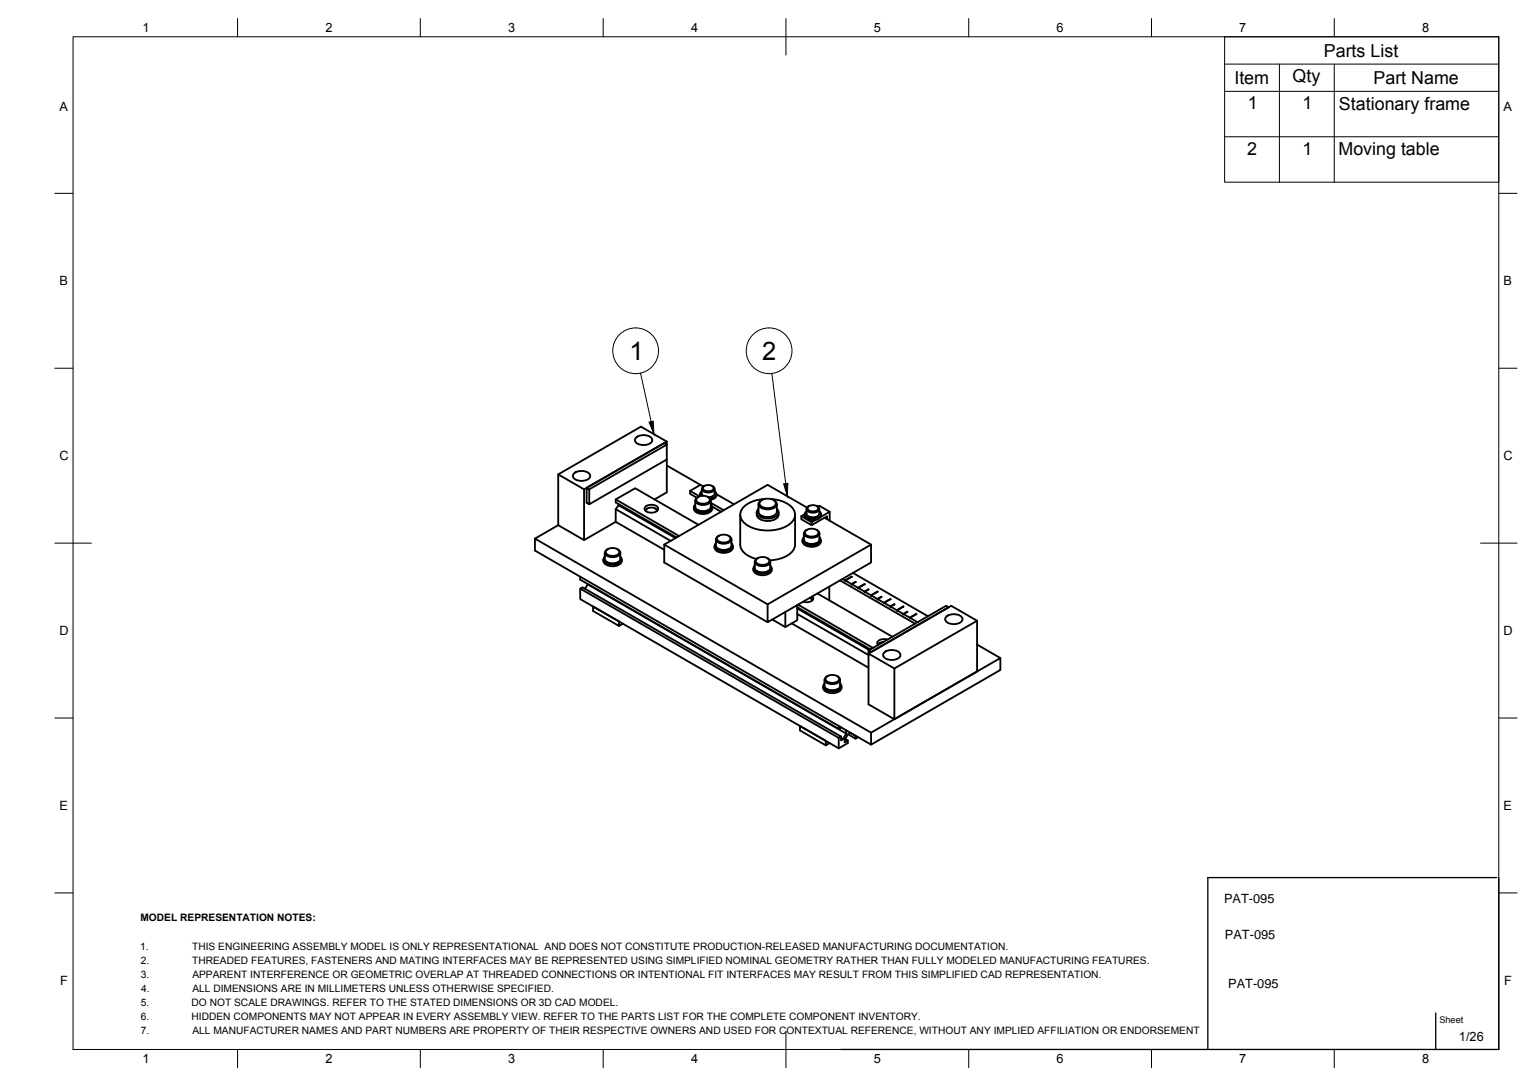
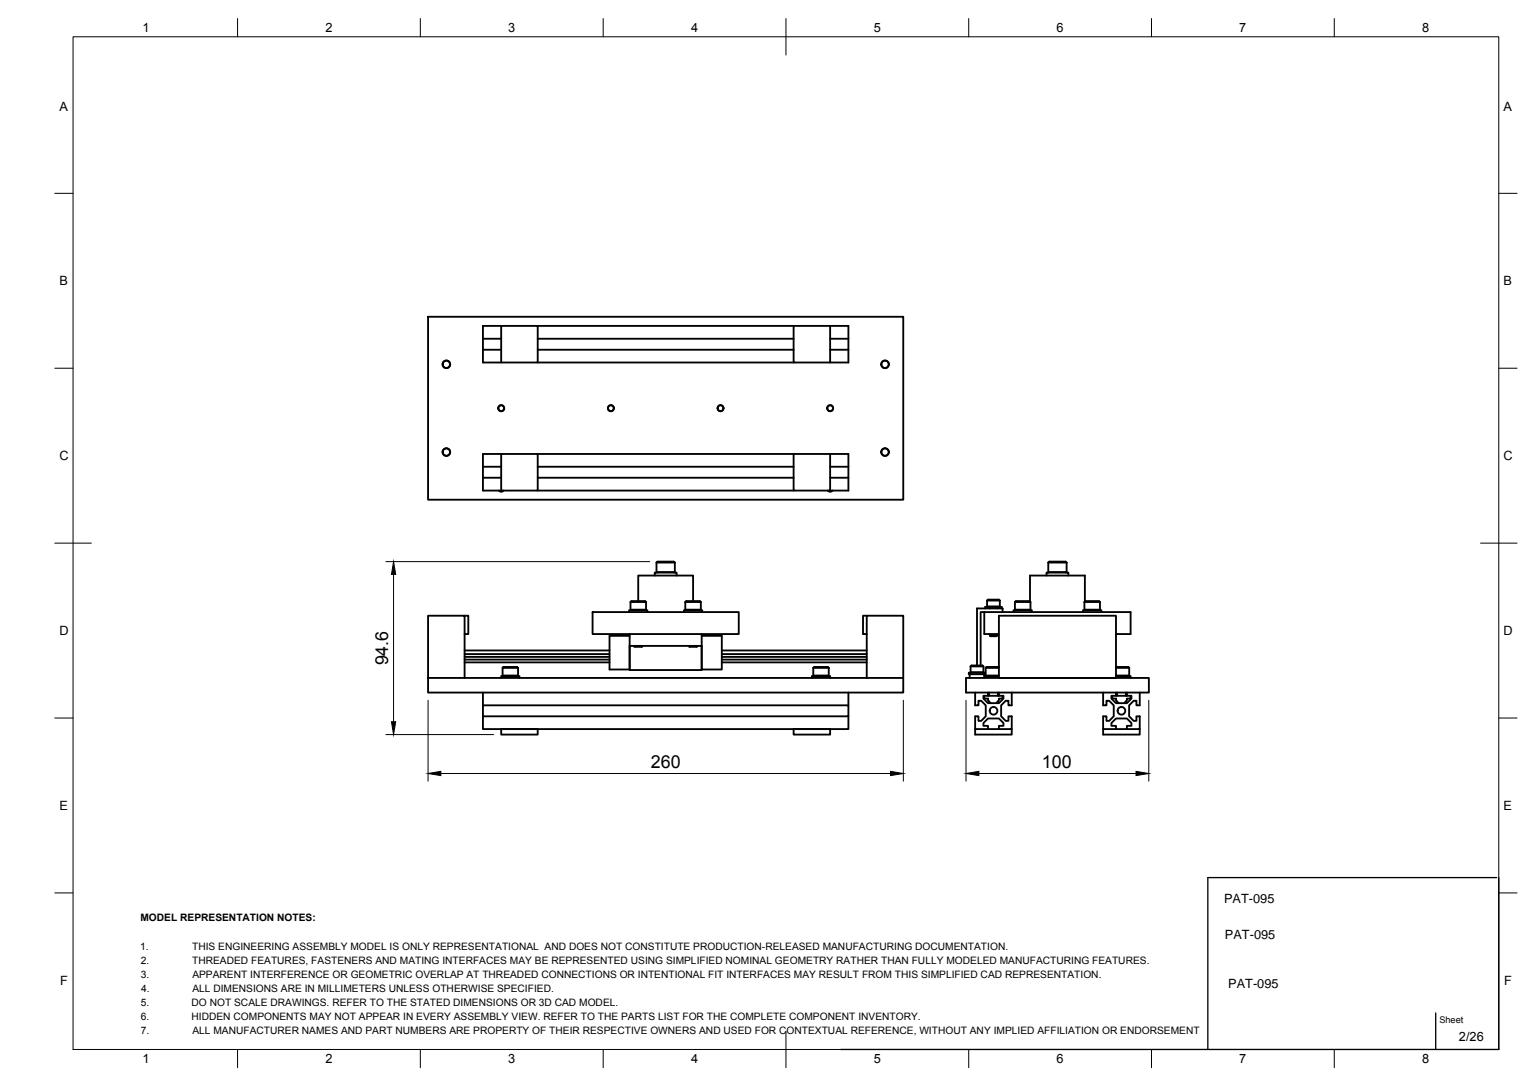
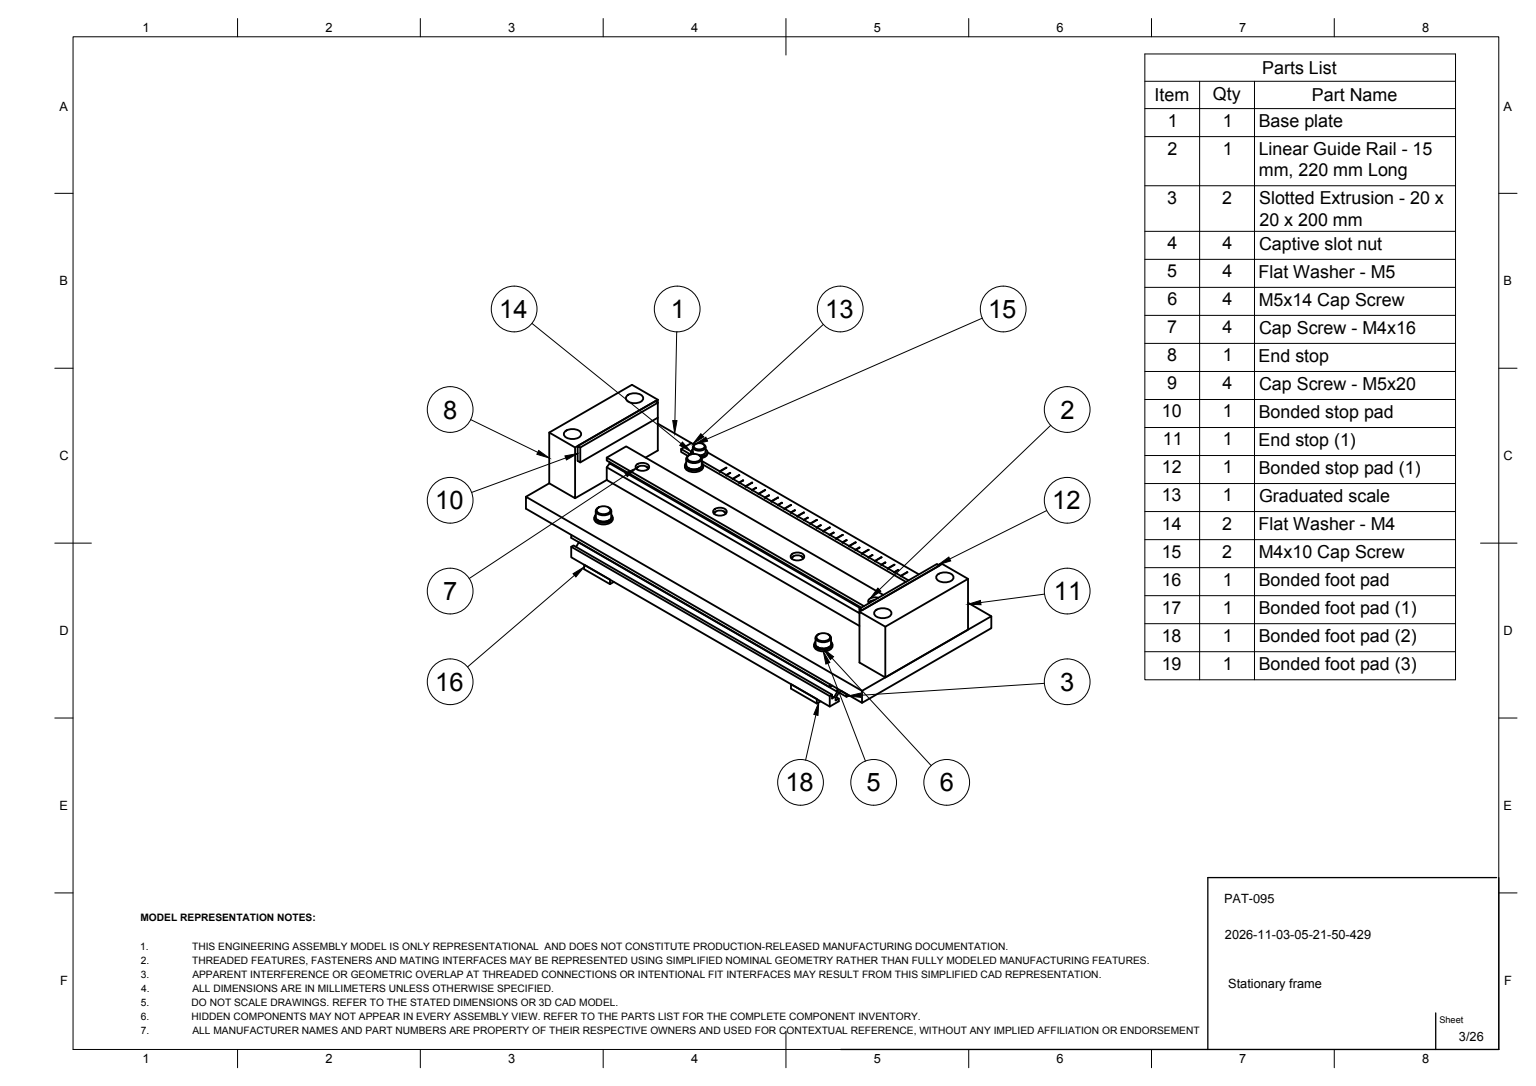
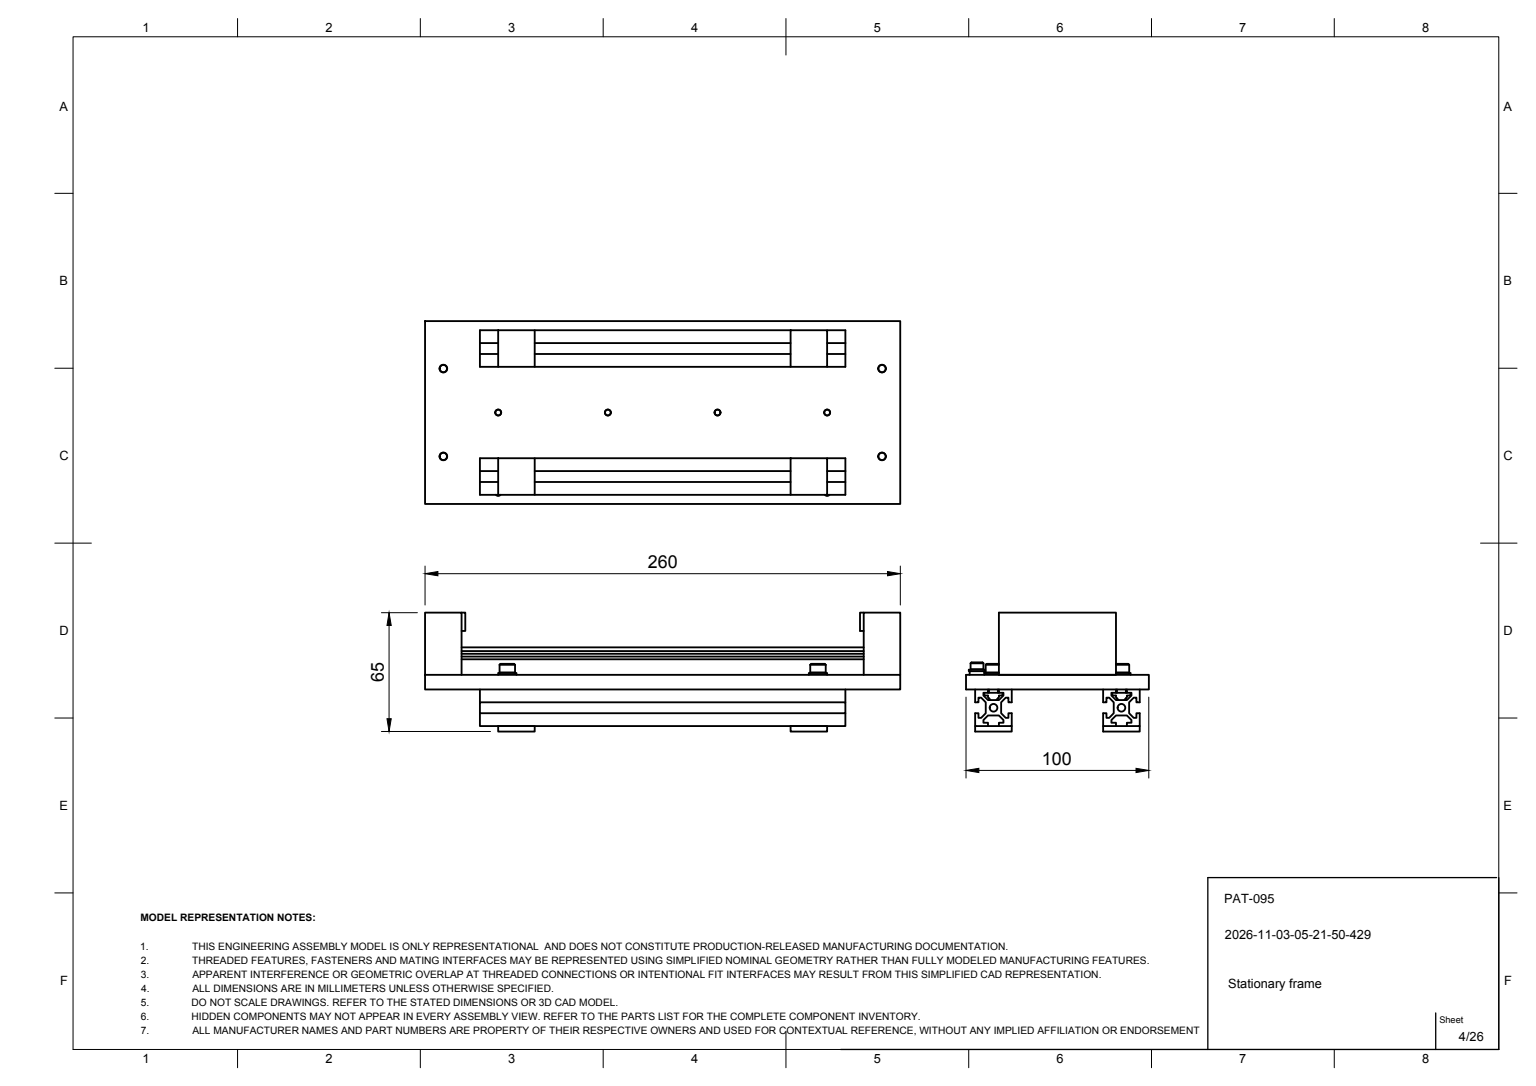
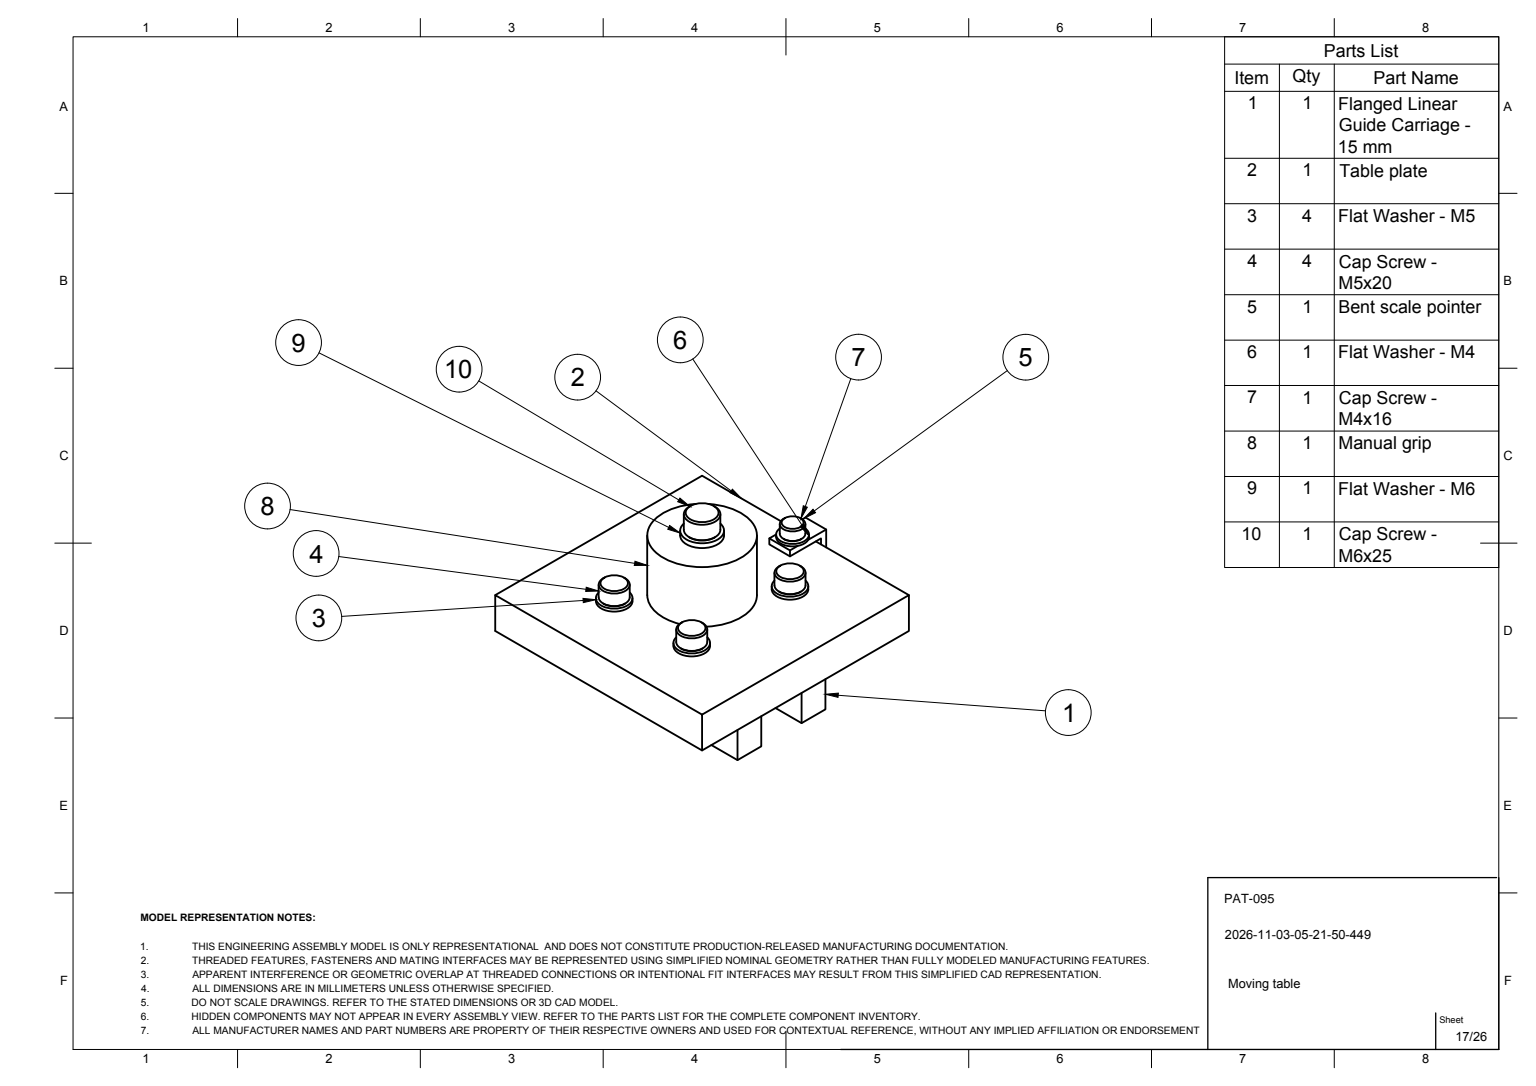
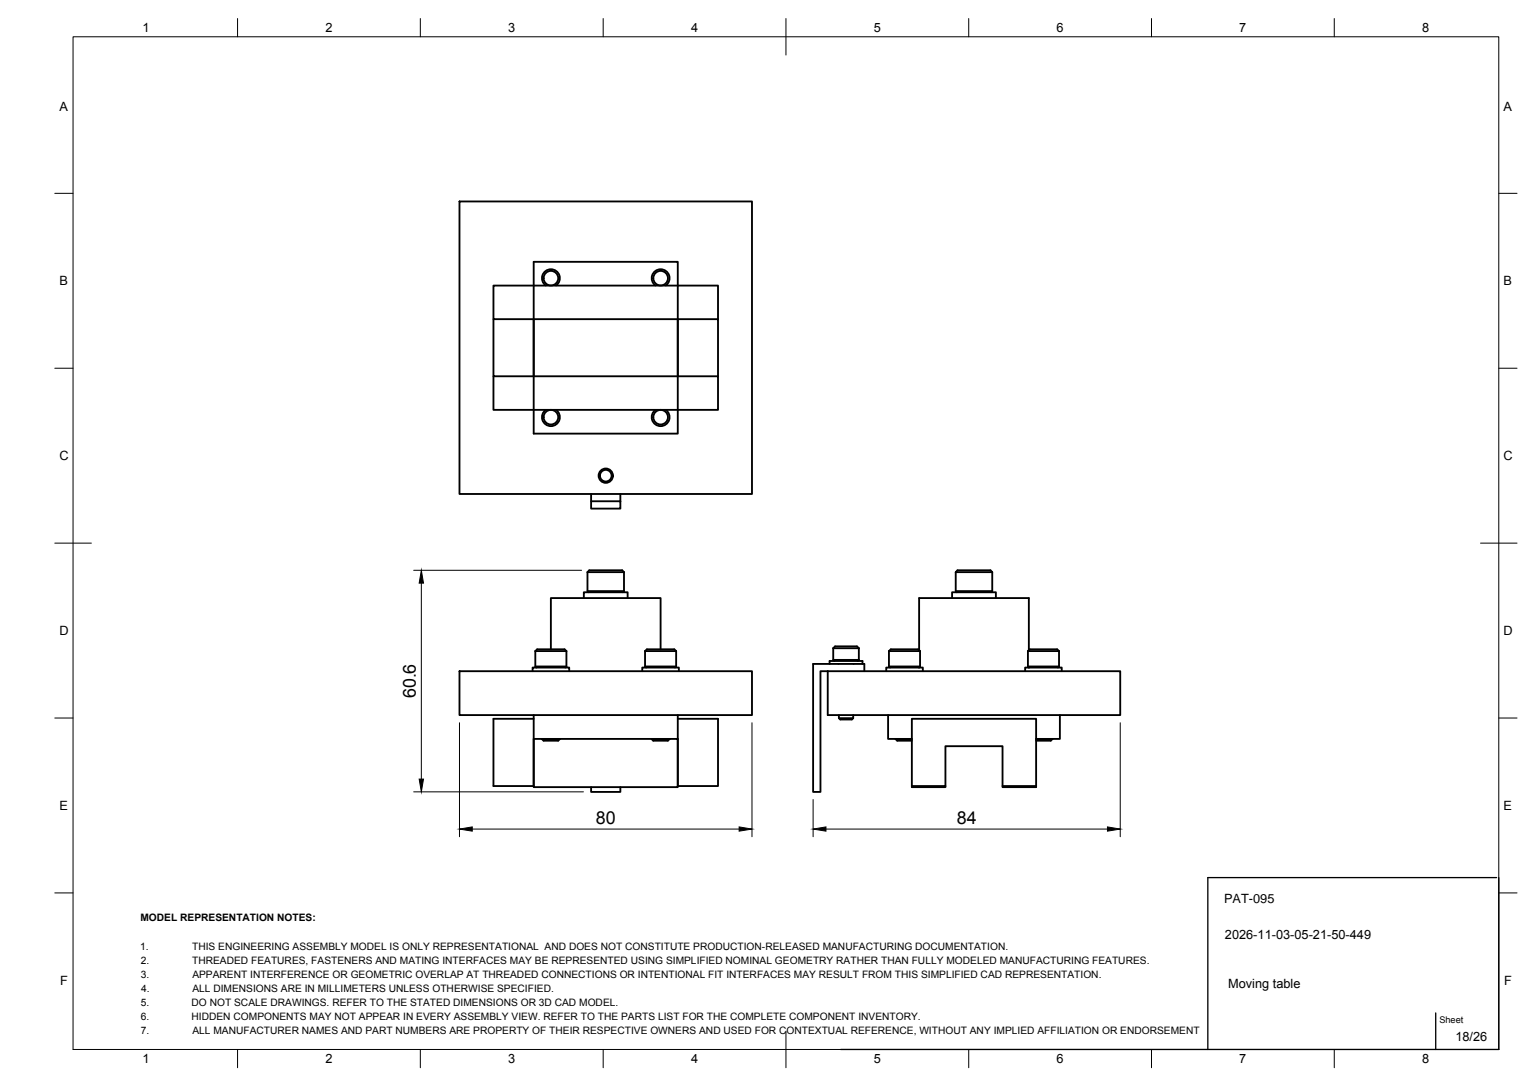
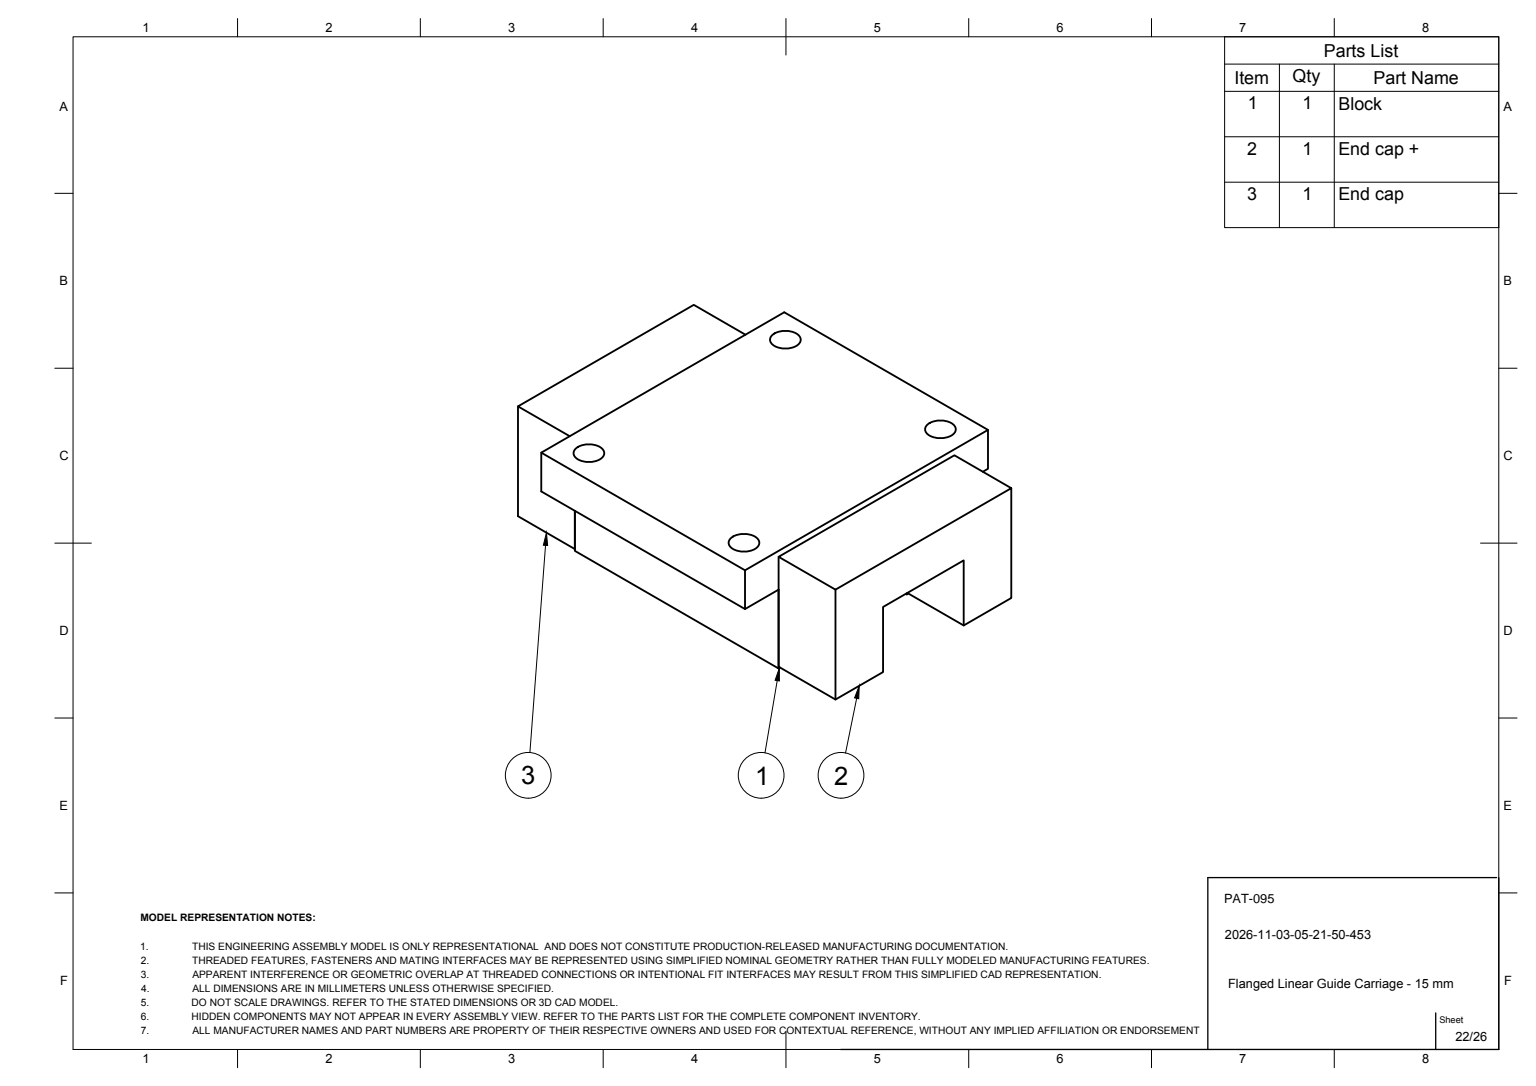
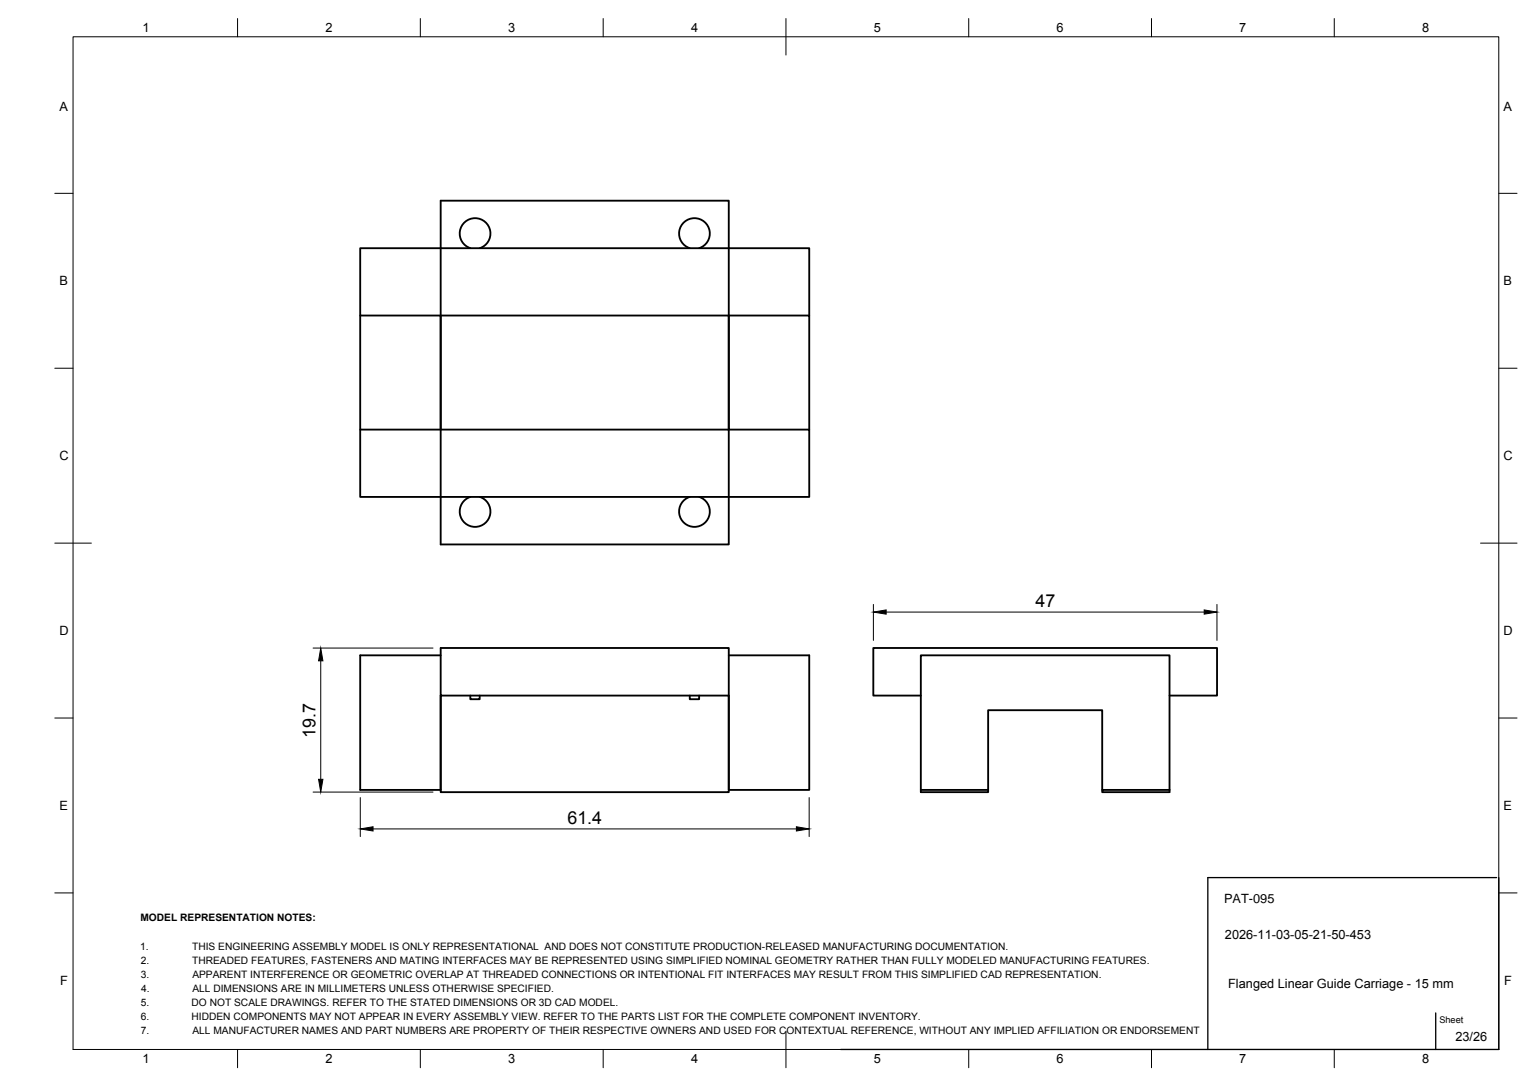
ISO-10303-21;
HEADER;
/* Generated by software containing ST-Developer
 * from STEP Tools, Inc. (www.steptools.com) 
 */

FILE_DESCRIPTION(
/* description */ ('Single-Axis Profile-Rail Linear Slide'),
/* implementation_level */ '2;1');

FILE_NAME(
/* name */ 'PAT-095',
/* time_stamp */ '2026-10-27T10:47:43-07:00',
/* author */ (''),
/* organization */ (''),
/* preprocessor_version */ 'ST-DEVELOPER v20.2',
/* originating_system */ 'Autodesk Translation Framework v15.17.0.0',
/* authorisation */ '');

FILE_SCHEMA (('AUTOMOTIVE_DESIGN { 1 0 10303 214 3 1 1 }'));
ENDSEC;

DATA;
#10=MECHANICAL_DESIGN_GEOMETRIC_PRESENTATION_REPRESENTATION('',(#329,#330,
#331,#332,#333,#334,#335,#336,#337,#338,#339,#340,#341,#342,#343,#344,#345,
#346,#347,#348,#349,#350,#351,#352,#353,#354,#355),#14478);
#11=ITEM_DEFINED_TRANSFORMATION($,$,#9393,#9454);
#12=ITEM_DEFINED_TRANSFORMATION($,$,#9432,#9455);
#13=ITEM_DEFINED_TRANSFORMATION($,$,#9443,#9456);
#14=ITEM_DEFINED_TRANSFORMATION($,$,#8921,#9531);
#15=ITEM_DEFINED_TRANSFORMATION($,$,#8970,#9532);
#16=ITEM_DEFINED_TRANSFORMATION($,$,#8991,#9533);
#17=ITEM_DEFINED_TRANSFORMATION($,$,#8998,#9534);
#18=ITEM_DEFINED_TRANSFORMATION($,$,#9019,#9535);
#19=ITEM_DEFINED_TRANSFORMATION($,$,#9026,#9536);
#20=ITEM_DEFINED_TRANSFORMATION($,$,#9155,#9537);
#21=ITEM_DEFINED_TRANSFORMATION($,$,#9162,#9538);
#22=ITEM_DEFINED_TRANSFORMATION($,$,#9169,#9539);
#23=ITEM_DEFINED_TRANSFORMATION($,$,#9176,#9540);
#24=ITEM_DEFINED_TRANSFORMATION($,$,#9183,#9541);
#25=ITEM_DEFINED_TRANSFORMATION($,$,#9226,#9542);
#26=ITEM_DEFINED_TRANSFORMATION($,$,#9226,#9543);
#27=ITEM_DEFINED_TRANSFORMATION($,$,#9276,#9544);
#28=ITEM_DEFINED_TRANSFORMATION($,$,#9457,#9545);
#29=ITEM_DEFINED_TRANSFORMATION($,$,#9297,#9546);
#30=ITEM_DEFINED_TRANSFORMATION($,$,#9276,#9547);
#31=ITEM_DEFINED_TRANSFORMATION($,$,#9457,#9548);
#32=ITEM_DEFINED_TRANSFORMATION($,$,#9297,#9549);
#33=ITEM_DEFINED_TRANSFORMATION($,$,#9276,#9550);
#34=ITEM_DEFINED_TRANSFORMATION($,$,#9457,#9551);
#35=ITEM_DEFINED_TRANSFORMATION($,$,#9297,#9552);
#36=ITEM_DEFINED_TRANSFORMATION($,$,#9276,#9553);
#37=ITEM_DEFINED_TRANSFORMATION($,$,#9457,#9554);
#38=ITEM_DEFINED_TRANSFORMATION($,$,#9297,#9555);
#39=ITEM_DEFINED_TRANSFORMATION($,$,#9505,#9556);
#40=ITEM_DEFINED_TRANSFORMATION($,$,#9505,#9557);
#41=ITEM_DEFINED_TRANSFORMATION($,$,#9505,#9558);
#42=ITEM_DEFINED_TRANSFORMATION($,$,#9505,#9559);
#43=ITEM_DEFINED_TRANSFORMATION($,$,#9468,#9560);
#44=ITEM_DEFINED_TRANSFORMATION($,$,#9468,#9561);
#45=ITEM_DEFINED_TRANSFORMATION($,$,#9468,#9562);
#46=ITEM_DEFINED_TRANSFORMATION($,$,#9468,#9563);
#47=ITEM_DEFINED_TRANSFORMATION($,$,#9494,#9564);
#48=ITEM_DEFINED_TRANSFORMATION($,$,#9321,#9565);
#49=ITEM_DEFINED_TRANSFORMATION($,$,#9494,#9566);
#50=ITEM_DEFINED_TRANSFORMATION($,$,#9321,#9567);
#51=ITEM_DEFINED_TRANSFORMATION($,$,#9346,#9603);
#52=ITEM_DEFINED_TRANSFORMATION($,$,#9371,#9604);
#53=ITEM_DEFINED_TRANSFORMATION($,$,#9383,#9605);
#54=ITEM_DEFINED_TRANSFORMATION($,$,#9392,#9606);
#55=ITEM_DEFINED_TRANSFORMATION($,$,#9457,#9607);
#56=ITEM_DEFINED_TRANSFORMATION($,$,#9468,#9608);
#57=ITEM_DEFINED_TRANSFORMATION($,$,#9457,#9609);
#58=ITEM_DEFINED_TRANSFORMATION($,$,#9468,#9610);
#59=ITEM_DEFINED_TRANSFORMATION($,$,#9457,#9611);
#60=ITEM_DEFINED_TRANSFORMATION($,$,#9468,#9612);
#61=ITEM_DEFINED_TRANSFORMATION($,$,#9457,#9613);
#62=ITEM_DEFINED_TRANSFORMATION($,$,#9468,#9614);
#63=ITEM_DEFINED_TRANSFORMATION($,$,#9494,#9615);
#64=ITEM_DEFINED_TRANSFORMATION($,$,#9505,#9616);
#65=ITEM_DEFINED_TRANSFORMATION($,$,#9568,#9617);
#66=ITEM_DEFINED_TRANSFORMATION($,$,#9577,#9618);
#67=ITEM_DEFINED_TRANSFORMATION($,$,#8920,#9619);
#68=ITEM_DEFINED_TRANSFORMATION($,$,#9345,#9620);
#69=(
REPRESENTATION_RELATIONSHIP($,$,#14625,#14624)
REPRESENTATION_RELATIONSHIP_WITH_TRANSFORMATION(#11)
SHAPE_REPRESENTATION_RELATIONSHIP()
);
#70=(
REPRESENTATION_RELATIONSHIP($,$,#14626,#14624)
REPRESENTATION_RELATIONSHIP_WITH_TRANSFORMATION(#12)
SHAPE_REPRESENTATION_RELATIONSHIP()
);
#71=(
REPRESENTATION_RELATIONSHIP($,$,#14627,#14624)
REPRESENTATION_RELATIONSHIP_WITH_TRANSFORMATION(#13)
SHAPE_REPRESENTATION_RELATIONSHIP()
);
#72=(
REPRESENTATION_RELATIONSHIP($,$,#14605,#14604)
REPRESENTATION_RELATIONSHIP_WITH_TRANSFORMATION(#14)
SHAPE_REPRESENTATION_RELATIONSHIP()
);
#73=(
REPRESENTATION_RELATIONSHIP($,$,#14606,#14604)
REPRESENTATION_RELATIONSHIP_WITH_TRANSFORMATION(#15)
SHAPE_REPRESENTATION_RELATIONSHIP()
);
#74=(
REPRESENTATION_RELATIONSHIP($,$,#14607,#14604)
REPRESENTATION_RELATIONSHIP_WITH_TRANSFORMATION(#16)
SHAPE_REPRESENTATION_RELATIONSHIP()
);
#75=(
REPRESENTATION_RELATIONSHIP($,$,#14608,#14604)
REPRESENTATION_RELATIONSHIP_WITH_TRANSFORMATION(#17)
SHAPE_REPRESENTATION_RELATIONSHIP()
);
#76=(
REPRESENTATION_RELATIONSHIP($,$,#14609,#14604)
REPRESENTATION_RELATIONSHIP_WITH_TRANSFORMATION(#18)
SHAPE_REPRESENTATION_RELATIONSHIP()
);
#77=(
REPRESENTATION_RELATIONSHIP($,$,#14610,#14604)
REPRESENTATION_RELATIONSHIP_WITH_TRANSFORMATION(#19)
SHAPE_REPRESENTATION_RELATIONSHIP()
);
#78=(
REPRESENTATION_RELATIONSHIP($,$,#14611,#14604)
REPRESENTATION_RELATIONSHIP_WITH_TRANSFORMATION(#20)
SHAPE_REPRESENTATION_RELATIONSHIP()
);
#79=(
REPRESENTATION_RELATIONSHIP($,$,#14612,#14604)
REPRESENTATION_RELATIONSHIP_WITH_TRANSFORMATION(#21)
SHAPE_REPRESENTATION_RELATIONSHIP()
);
#80=(
REPRESENTATION_RELATIONSHIP($,$,#14613,#14604)
REPRESENTATION_RELATIONSHIP_WITH_TRANSFORMATION(#22)
SHAPE_REPRESENTATION_RELATIONSHIP()
);
#81=(
REPRESENTATION_RELATIONSHIP($,$,#14614,#14604)
REPRESENTATION_RELATIONSHIP_WITH_TRANSFORMATION(#23)
SHAPE_REPRESENTATION_RELATIONSHIP()
);
#82=(
REPRESENTATION_RELATIONSHIP($,$,#14615,#14604)
REPRESENTATION_RELATIONSHIP_WITH_TRANSFORMATION(#24)
SHAPE_REPRESENTATION_RELATIONSHIP()
);
#83=(
REPRESENTATION_RELATIONSHIP($,$,#14616,#14604)
REPRESENTATION_RELATIONSHIP_WITH_TRANSFORMATION(#25)
SHAPE_REPRESENTATION_RELATIONSHIP()
);
#84=(
REPRESENTATION_RELATIONSHIP($,$,#14616,#14604)
REPRESENTATION_RELATIONSHIP_WITH_TRANSFORMATION(#26)
SHAPE_REPRESENTATION_RELATIONSHIP()
);
#85=(
REPRESENTATION_RELATIONSHIP($,$,#14617,#14604)
REPRESENTATION_RELATIONSHIP_WITH_TRANSFORMATION(#27)
SHAPE_REPRESENTATION_RELATIONSHIP()
);
#86=(
REPRESENTATION_RELATIONSHIP($,$,#14628,#14604)
REPRESENTATION_RELATIONSHIP_WITH_TRANSFORMATION(#28)
SHAPE_REPRESENTATION_RELATIONSHIP()
);
#87=(
REPRESENTATION_RELATIONSHIP($,$,#14618,#14604)
REPRESENTATION_RELATIONSHIP_WITH_TRANSFORMATION(#29)
SHAPE_REPRESENTATION_RELATIONSHIP()
);
#88=(
REPRESENTATION_RELATIONSHIP($,$,#14617,#14604)
REPRESENTATION_RELATIONSHIP_WITH_TRANSFORMATION(#30)
SHAPE_REPRESENTATION_RELATIONSHIP()
);
#89=(
REPRESENTATION_RELATIONSHIP($,$,#14628,#14604)
REPRESENTATION_RELATIONSHIP_WITH_TRANSFORMATION(#31)
SHAPE_REPRESENTATION_RELATIONSHIP()
);
#90=(
REPRESENTATION_RELATIONSHIP($,$,#14618,#14604)
REPRESENTATION_RELATIONSHIP_WITH_TRANSFORMATION(#32)
SHAPE_REPRESENTATION_RELATIONSHIP()
);
#91=(
REPRESENTATION_RELATIONSHIP($,$,#14617,#14604)
REPRESENTATION_RELATIONSHIP_WITH_TRANSFORMATION(#33)
SHAPE_REPRESENTATION_RELATIONSHIP()
);
#92=(
REPRESENTATION_RELATIONSHIP($,$,#14628,#14604)
REPRESENTATION_RELATIONSHIP_WITH_TRANSFORMATION(#34)
SHAPE_REPRESENTATION_RELATIONSHIP()
);
#93=(
REPRESENTATION_RELATIONSHIP($,$,#14618,#14604)
REPRESENTATION_RELATIONSHIP_WITH_TRANSFORMATION(#35)
SHAPE_REPRESENTATION_RELATIONSHIP()
);
#94=(
REPRESENTATION_RELATIONSHIP($,$,#14617,#14604)
REPRESENTATION_RELATIONSHIP_WITH_TRANSFORMATION(#36)
SHAPE_REPRESENTATION_RELATIONSHIP()
);
#95=(
REPRESENTATION_RELATIONSHIP($,$,#14628,#14604)
REPRESENTATION_RELATIONSHIP_WITH_TRANSFORMATION(#37)
SHAPE_REPRESENTATION_RELATIONSHIP()
);
#96=(
REPRESENTATION_RELATIONSHIP($,$,#14618,#14604)
REPRESENTATION_RELATIONSHIP_WITH_TRANSFORMATION(#38)
SHAPE_REPRESENTATION_RELATIONSHIP()
);
#97=(
REPRESENTATION_RELATIONSHIP($,$,#14631,#14604)
REPRESENTATION_RELATIONSHIP_WITH_TRANSFORMATION(#39)
SHAPE_REPRESENTATION_RELATIONSHIP()
);
#98=(
REPRESENTATION_RELATIONSHIP($,$,#14631,#14604)
REPRESENTATION_RELATIONSHIP_WITH_TRANSFORMATION(#40)
SHAPE_REPRESENTATION_RELATIONSHIP()
);
#99=(
REPRESENTATION_RELATIONSHIP($,$,#14631,#14604)
REPRESENTATION_RELATIONSHIP_WITH_TRANSFORMATION(#41)
SHAPE_REPRESENTATION_RELATIONSHIP()
);
#100=(
REPRESENTATION_RELATIONSHIP($,$,#14631,#14604)
REPRESENTATION_RELATIONSHIP_WITH_TRANSFORMATION(#42)
SHAPE_REPRESENTATION_RELATIONSHIP()
);
#101=(
REPRESENTATION_RELATIONSHIP($,$,#14629,#14604)
REPRESENTATION_RELATIONSHIP_WITH_TRANSFORMATION(#43)
SHAPE_REPRESENTATION_RELATIONSHIP()
);
#102=(
REPRESENTATION_RELATIONSHIP($,$,#14629,#14604)
REPRESENTATION_RELATIONSHIP_WITH_TRANSFORMATION(#44)
SHAPE_REPRESENTATION_RELATIONSHIP()
);
#103=(
REPRESENTATION_RELATIONSHIP($,$,#14629,#14604)
REPRESENTATION_RELATIONSHIP_WITH_TRANSFORMATION(#45)
SHAPE_REPRESENTATION_RELATIONSHIP()
);
#104=(
REPRESENTATION_RELATIONSHIP($,$,#14629,#14604)
REPRESENTATION_RELATIONSHIP_WITH_TRANSFORMATION(#46)
SHAPE_REPRESENTATION_RELATIONSHIP()
);
#105=(
REPRESENTATION_RELATIONSHIP($,$,#14630,#14604)
REPRESENTATION_RELATIONSHIP_WITH_TRANSFORMATION(#47)
SHAPE_REPRESENTATION_RELATIONSHIP()
);
#106=(
REPRESENTATION_RELATIONSHIP($,$,#14619,#14604)
REPRESENTATION_RELATIONSHIP_WITH_TRANSFORMATION(#48)
SHAPE_REPRESENTATION_RELATIONSHIP()
);
#107=(
REPRESENTATION_RELATIONSHIP($,$,#14630,#14604)
REPRESENTATION_RELATIONSHIP_WITH_TRANSFORMATION(#49)
SHAPE_REPRESENTATION_RELATIONSHIP()
);
#108=(
REPRESENTATION_RELATIONSHIP($,$,#14619,#14604)
REPRESENTATION_RELATIONSHIP_WITH_TRANSFORMATION(#50)
SHAPE_REPRESENTATION_RELATIONSHIP()
);
#109=(
REPRESENTATION_RELATIONSHIP($,$,#14621,#14620)
REPRESENTATION_RELATIONSHIP_WITH_TRANSFORMATION(#51)
SHAPE_REPRESENTATION_RELATIONSHIP()
);
#110=(
REPRESENTATION_RELATIONSHIP($,$,#14622,#14620)
REPRESENTATION_RELATIONSHIP_WITH_TRANSFORMATION(#52)
SHAPE_REPRESENTATION_RELATIONSHIP()
);
#111=(
REPRESENTATION_RELATIONSHIP($,$,#14623,#14620)
REPRESENTATION_RELATIONSHIP_WITH_TRANSFORMATION(#53)
SHAPE_REPRESENTATION_RELATIONSHIP()
);
#112=(
REPRESENTATION_RELATIONSHIP($,$,#14624,#14620)
REPRESENTATION_RELATIONSHIP_WITH_TRANSFORMATION(#54)
SHAPE_REPRESENTATION_RELATIONSHIP()
);
#113=(
REPRESENTATION_RELATIONSHIP($,$,#14628,#14620)
REPRESENTATION_RELATIONSHIP_WITH_TRANSFORMATION(#55)
SHAPE_REPRESENTATION_RELATIONSHIP()
);
#114=(
REPRESENTATION_RELATIONSHIP($,$,#14629,#14620)
REPRESENTATION_RELATIONSHIP_WITH_TRANSFORMATION(#56)
SHAPE_REPRESENTATION_RELATIONSHIP()
);
#115=(
REPRESENTATION_RELATIONSHIP($,$,#14628,#14620)
REPRESENTATION_RELATIONSHIP_WITH_TRANSFORMATION(#57)
SHAPE_REPRESENTATION_RELATIONSHIP()
);
#116=(
REPRESENTATION_RELATIONSHIP($,$,#14629,#14620)
REPRESENTATION_RELATIONSHIP_WITH_TRANSFORMATION(#58)
SHAPE_REPRESENTATION_RELATIONSHIP()
);
#117=(
REPRESENTATION_RELATIONSHIP($,$,#14628,#14620)
REPRESENTATION_RELATIONSHIP_WITH_TRANSFORMATION(#59)
SHAPE_REPRESENTATION_RELATIONSHIP()
);
#118=(
REPRESENTATION_RELATIONSHIP($,$,#14629,#14620)
REPRESENTATION_RELATIONSHIP_WITH_TRANSFORMATION(#60)
SHAPE_REPRESENTATION_RELATIONSHIP()
);
#119=(
REPRESENTATION_RELATIONSHIP($,$,#14628,#14620)
REPRESENTATION_RELATIONSHIP_WITH_TRANSFORMATION(#61)
SHAPE_REPRESENTATION_RELATIONSHIP()
);
#120=(
REPRESENTATION_RELATIONSHIP($,$,#14629,#14620)
REPRESENTATION_RELATIONSHIP_WITH_TRANSFORMATION(#62)
SHAPE_REPRESENTATION_RELATIONSHIP()
);
#121=(
REPRESENTATION_RELATIONSHIP($,$,#14630,#14620)
REPRESENTATION_RELATIONSHIP_WITH_TRANSFORMATION(#63)
SHAPE_REPRESENTATION_RELATIONSHIP()
);
#122=(
REPRESENTATION_RELATIONSHIP($,$,#14631,#14620)
REPRESENTATION_RELATIONSHIP_WITH_TRANSFORMATION(#64)
SHAPE_REPRESENTATION_RELATIONSHIP()
);
#123=(
REPRESENTATION_RELATIONSHIP($,$,#14632,#14620)
REPRESENTATION_RELATIONSHIP_WITH_TRANSFORMATION(#65)
SHAPE_REPRESENTATION_RELATIONSHIP()
);
#124=(
REPRESENTATION_RELATIONSHIP($,$,#14633,#14620)
REPRESENTATION_RELATIONSHIP_WITH_TRANSFORMATION(#66)
SHAPE_REPRESENTATION_RELATIONSHIP()
);
#125=(
REPRESENTATION_RELATIONSHIP($,$,#14604,#14603)
REPRESENTATION_RELATIONSHIP_WITH_TRANSFORMATION(#67)
SHAPE_REPRESENTATION_RELATIONSHIP()
);
#126=(
REPRESENTATION_RELATIONSHIP($,$,#14620,#14603)
REPRESENTATION_RELATIONSHIP_WITH_TRANSFORMATION(#68)
SHAPE_REPRESENTATION_RELATIONSHIP()
);
#127=CONTEXT_DEPENDENT_SHAPE_REPRESENTATION(#69,#14539);
#128=CONTEXT_DEPENDENT_SHAPE_REPRESENTATION(#70,#14540);
#129=CONTEXT_DEPENDENT_SHAPE_REPRESENTATION(#71,#14541);
#130=CONTEXT_DEPENDENT_SHAPE_REPRESENTATION(#72,#14546);
#131=CONTEXT_DEPENDENT_SHAPE_REPRESENTATION(#73,#14547);
#132=CONTEXT_DEPENDENT_SHAPE_REPRESENTATION(#74,#14548);
#133=CONTEXT_DEPENDENT_SHAPE_REPRESENTATION(#75,#14549);
#134=CONTEXT_DEPENDENT_SHAPE_REPRESENTATION(#76,#14550);
#135=CONTEXT_DEPENDENT_SHAPE_REPRESENTATION(#77,#14551);
#136=CONTEXT_DEPENDENT_SHAPE_REPRESENTATION(#78,#14552);
#137=CONTEXT_DEPENDENT_SHAPE_REPRESENTATION(#79,#14553);
#138=CONTEXT_DEPENDENT_SHAPE_REPRESENTATION(#80,#14554);
#139=CONTEXT_DEPENDENT_SHAPE_REPRESENTATION(#81,#14555);
#140=CONTEXT_DEPENDENT_SHAPE_REPRESENTATION(#82,#14556);
#141=CONTEXT_DEPENDENT_SHAPE_REPRESENTATION(#83,#14557);
#142=CONTEXT_DEPENDENT_SHAPE_REPRESENTATION(#84,#14558);
#143=CONTEXT_DEPENDENT_SHAPE_REPRESENTATION(#85,#14559);
#144=CONTEXT_DEPENDENT_SHAPE_REPRESENTATION(#86,#14560);
#145=CONTEXT_DEPENDENT_SHAPE_REPRESENTATION(#87,#14561);
#146=CONTEXT_DEPENDENT_SHAPE_REPRESENTATION(#88,#14562);
#147=CONTEXT_DEPENDENT_SHAPE_REPRESENTATION(#89,#14563);
#148=CONTEXT_DEPENDENT_SHAPE_REPRESENTATION(#90,#14564);
#149=CONTEXT_DEPENDENT_SHAPE_REPRESENTATION(#91,#14565);
#150=CONTEXT_DEPENDENT_SHAPE_REPRESENTATION(#92,#14566);
#151=CONTEXT_DEPENDENT_SHAPE_REPRESENTATION(#93,#14567);
#152=CONTEXT_DEPENDENT_SHAPE_REPRESENTATION(#94,#14568);
#153=CONTEXT_DEPENDENT_SHAPE_REPRESENTATION(#95,#14569);
#154=CONTEXT_DEPENDENT_SHAPE_REPRESENTATION(#96,#14570);
#155=CONTEXT_DEPENDENT_SHAPE_REPRESENTATION(#97,#14571);
#156=CONTEXT_DEPENDENT_SHAPE_REPRESENTATION(#98,#14572);
#157=CONTEXT_DEPENDENT_SHAPE_REPRESENTATION(#99,#14573);
#158=CONTEXT_DEPENDENT_SHAPE_REPRESENTATION(#100,#14574);
#159=CONTEXT_DEPENDENT_SHAPE_REPRESENTATION(#101,#14575);
#160=CONTEXT_DEPENDENT_SHAPE_REPRESENTATION(#102,#14576);
#161=CONTEXT_DEPENDENT_SHAPE_REPRESENTATION(#103,#14577);
#162=CONTEXT_DEPENDENT_SHAPE_REPRESENTATION(#104,#14578);
#163=CONTEXT_DEPENDENT_SHAPE_REPRESENTATION(#105,#14579);
#164=CONTEXT_DEPENDENT_SHAPE_REPRESENTATION(#106,#14580);
#165=CONTEXT_DEPENDENT_SHAPE_REPRESENTATION(#107,#14581);
#166=CONTEXT_DEPENDENT_SHAPE_REPRESENTATION(#108,#14582);
#167=CONTEXT_DEPENDENT_SHAPE_REPRESENTATION(#109,#14585);
#168=CONTEXT_DEPENDENT_SHAPE_REPRESENTATION(#110,#14586);
#169=CONTEXT_DEPENDENT_SHAPE_REPRESENTATION(#111,#14587);
#170=CONTEXT_DEPENDENT_SHAPE_REPRESENTATION(#112,#14588);
#171=CONTEXT_DEPENDENT_SHAPE_REPRESENTATION(#113,#14589);
#172=CONTEXT_DEPENDENT_SHAPE_REPRESENTATION(#114,#14590);
#173=CONTEXT_DEPENDENT_SHAPE_REPRESENTATION(#115,#14591);
#174=CONTEXT_DEPENDENT_SHAPE_REPRESENTATION(#116,#14592);
#175=CONTEXT_DEPENDENT_SHAPE_REPRESENTATION(#117,#14593);
#176=CONTEXT_DEPENDENT_SHAPE_REPRESENTATION(#118,#14594);
#177=CONTEXT_DEPENDENT_SHAPE_REPRESENTATION(#119,#14595);
#178=CONTEXT_DEPENDENT_SHAPE_REPRESENTATION(#120,#14596);
#179=CONTEXT_DEPENDENT_SHAPE_REPRESENTATION(#121,#14597);
#180=CONTEXT_DEPENDENT_SHAPE_REPRESENTATION(#122,#14598);
#181=CONTEXT_DEPENDENT_SHAPE_REPRESENTATION(#123,#14599);
#182=CONTEXT_DEPENDENT_SHAPE_REPRESENTATION(#124,#14600);
#183=CONTEXT_DEPENDENT_SHAPE_REPRESENTATION(#125,#14601);
#184=CONTEXT_DEPENDENT_SHAPE_REPRESENTATION(#126,#14602);
#185=NEXT_ASSEMBLY_USAGE_OCCURRENCE('Block:1','Block:1','Block:1',#14656,
#14657,'Block:1');
#186=NEXT_ASSEMBLY_USAGE_OCCURRENCE('End cap +:1','End cap +:1',
'End cap +:1',#14656,#14658,'End cap +:1');
#187=NEXT_ASSEMBLY_USAGE_OCCURRENCE('End cap:1','End cap:1','End cap:1',
#14656,#14659,'End cap:1');
#188=NEXT_ASSEMBLY_USAGE_OCCURRENCE('Base plate:1','Base plate:1',
'Base plate:1',#14636,#14637,'Base plate:1');
#189=NEXT_ASSEMBLY_USAGE_OCCURRENCE('End stop:1','End stop:1',
'End stop:1',#14636,#14638,'End stop:1');
#190=NEXT_ASSEMBLY_USAGE_OCCURRENCE('Bonded stop pad:1',
'Bonded stop pad:1','Bonded stop pad:1',#14636,#14639,
'Bonded stop pad:1');
#191=NEXT_ASSEMBLY_USAGE_OCCURRENCE('End stop (1):1','End stop (1):1',
'End stop (1):1',#14636,#14640,'End stop (1):1');
#192=NEXT_ASSEMBLY_USAGE_OCCURRENCE('Bonded stop pad (1):1',
'Bonded stop pad (1):1','Bonded stop pad (1):1',#14636,#14641,
'Bonded stop pad (1):1');
#193=NEXT_ASSEMBLY_USAGE_OCCURRENCE('Graduated scale:1',
'Graduated scale:1','Graduated scale:1',#14636,#14642,
'Graduated scale:1');
#194=NEXT_ASSEMBLY_USAGE_OCCURRENCE('Bonded foot pad:1',
'Bonded foot pad:1','Bonded foot pad:1',#14636,#14643,
'Bonded foot pad:1');
#195=NEXT_ASSEMBLY_USAGE_OCCURRENCE('Bonded foot pad (1):1',
'Bonded foot pad (1):1','Bonded foot pad (1):1',#14636,#14644,
'Bonded foot pad (1):1');
#196=NEXT_ASSEMBLY_USAGE_OCCURRENCE('Bonded foot pad (2):1',
'Bonded foot pad (2):1','Bonded foot pad (2):1',#14636,#14645,
'Bonded foot pad (2):1');
#197=NEXT_ASSEMBLY_USAGE_OCCURRENCE('Bonded foot pad (3):1',
'Bonded foot pad (3):1','Bonded foot pad (3):1',#14636,#14646,
'Bonded foot pad (3):1');
#198=NEXT_ASSEMBLY_USAGE_OCCURRENCE(
'Linear Guide Rail - 15 mm, 220 mm Long:2',
'Linear Guide Rail - 15 mm, 220 mm Long:2',
'Linear Guide Rail - 15 mm, 220 mm Long:2',#14636,#14647,
'Linear Guide Rail - 15 mm, 220 mm Long:2');
#199=NEXT_ASSEMBLY_USAGE_OCCURRENCE(
'Slotted Extrusion - 20 x 20 x 200 mm:2',
'Slotted Extrusion - 20 x 20 x 200 mm:2',
'Slotted Extrusion - 20 x 20 x 200 mm:2',#14636,#14648,
'Slotted Extrusion - 20 x 20 x 200 mm:2');
#200=NEXT_ASSEMBLY_USAGE_OCCURRENCE(
'Slotted Extrusion - 20 x 20 x 200 mm:3',
'Slotted Extrusion - 20 x 20 x 200 mm:3',
'Slotted Extrusion - 20 x 20 x 200 mm:3',#14636,#14648,
'Slotted Extrusion - 20 x 20 x 200 mm:3');
#201=NEXT_ASSEMBLY_USAGE_OCCURRENCE('Captive slot nut:2',
'Captive slot nut:2','Captive slot nut:2',#14636,#14649,
'Captive slot nut:2');
#202=NEXT_ASSEMBLY_USAGE_OCCURRENCE('Flat Washer - M5:2',
'Flat Washer - M5:2','Flat Washer - M5:2',#14636,#14660,
'Flat Washer - M5:2');
#203=NEXT_ASSEMBLY_USAGE_OCCURRENCE('M5x14 Cap Screw:2',
'M5x14 Cap Screw:2','M5x14 Cap Screw:2',#14636,#14650,
'M5x14 Cap Screw:2');
#204=NEXT_ASSEMBLY_USAGE_OCCURRENCE('Captive slot nut:3',
'Captive slot nut:3','Captive slot nut:3',#14636,#14649,
'Captive slot nut:3');
#205=NEXT_ASSEMBLY_USAGE_OCCURRENCE('Flat Washer - M5:3',
'Flat Washer - M5:3','Flat Washer - M5:3',#14636,#14660,
'Flat Washer - M5:3');
#206=NEXT_ASSEMBLY_USAGE_OCCURRENCE('M5x14 Cap Screw:3',
'M5x14 Cap Screw:3','M5x14 Cap Screw:3',#14636,#14650,
'M5x14 Cap Screw:3');
#207=NEXT_ASSEMBLY_USAGE_OCCURRENCE('Captive slot nut:4',
'Captive slot nut:4','Captive slot nut:4',#14636,#14649,
'Captive slot nut:4');
#208=NEXT_ASSEMBLY_USAGE_OCCURRENCE('Flat Washer - M5:4',
'Flat Washer - M5:4','Flat Washer - M5:4',#14636,#14660,
'Flat Washer - M5:4');
#209=NEXT_ASSEMBLY_USAGE_OCCURRENCE('M5x14 Cap Screw:4',
'M5x14 Cap Screw:4','M5x14 Cap Screw:4',#14636,#14650,
'M5x14 Cap Screw:4');
#210=NEXT_ASSEMBLY_USAGE_OCCURRENCE('Captive slot nut:5',
'Captive slot nut:5','Captive slot nut:5',#14636,#14649,
'Captive slot nut:5');
#211=NEXT_ASSEMBLY_USAGE_OCCURRENCE('Flat Washer - M5:5',
'Flat Washer - M5:5','Flat Washer - M5:5',#14636,#14660,
'Flat Washer - M5:5');
#212=NEXT_ASSEMBLY_USAGE_OCCURRENCE('M5x14 Cap Screw:5',
'M5x14 Cap Screw:5','M5x14 Cap Screw:5',#14636,#14650,
'M5x14 Cap Screw:5');
#213=NEXT_ASSEMBLY_USAGE_OCCURRENCE('Cap Screw - M4x16:2',
'Cap Screw - M4x16:2','Cap Screw - M4x16:2',#14636,#14663,
'Cap Screw - M4x16:2');
#214=NEXT_ASSEMBLY_USAGE_OCCURRENCE('Cap Screw - M4x16:3',
'Cap Screw - M4x16:3','Cap Screw - M4x16:3',#14636,#14663,
'Cap Screw - M4x16:3');
#215=NEXT_ASSEMBLY_USAGE_OCCURRENCE('Cap Screw - M4x16:4',
'Cap Screw - M4x16:4','Cap Screw - M4x16:4',#14636,#14663,
'Cap Screw - M4x16:4');
#216=NEXT_ASSEMBLY_USAGE_OCCURRENCE('Cap Screw - M4x16:5',
'Cap Screw - M4x16:5','Cap Screw - M4x16:5',#14636,#14663,
'Cap Screw - M4x16:5');
#217=NEXT_ASSEMBLY_USAGE_OCCURRENCE('Cap Screw - M5x20:6',
'Cap Screw - M5x20:6','Cap Screw - M5x20:6',#14636,#14661,
'Cap Screw - M5x20:6');
#218=NEXT_ASSEMBLY_USAGE_OCCURRENCE('Cap Screw - M5x20:7',
'Cap Screw - M5x20:7','Cap Screw - M5x20:7',#14636,#14661,
'Cap Screw - M5x20:7');
#219=NEXT_ASSEMBLY_USAGE_OCCURRENCE('Cap Screw - M5x20:8',
'Cap Screw - M5x20:8','Cap Screw - M5x20:8',#14636,#14661,
'Cap Screw - M5x20:8');
#220=NEXT_ASSEMBLY_USAGE_OCCURRENCE('Cap Screw - M5x20:9',
'Cap Screw - M5x20:9','Cap Screw - M5x20:9',#14636,#14661,
'Cap Screw - M5x20:9');
#221=NEXT_ASSEMBLY_USAGE_OCCURRENCE('Flat Washer - M4:2',
'Flat Washer - M4:2','Flat Washer - M4:2',#14636,#14662,
'Flat Washer - M4:2');
#222=NEXT_ASSEMBLY_USAGE_OCCURRENCE('M4x10 Cap Screw:2',
'M4x10 Cap Screw:2','M4x10 Cap Screw:2',#14636,#14651,
'M4x10 Cap Screw:2');
#223=NEXT_ASSEMBLY_USAGE_OCCURRENCE('Flat Washer - M4:3',
'Flat Washer - M4:3','Flat Washer - M4:3',#14636,#14662,
'Flat Washer - M4:3');
#224=NEXT_ASSEMBLY_USAGE_OCCURRENCE('M4x10 Cap Screw:3',
'M4x10 Cap Screw:3','M4x10 Cap Screw:3',#14636,#14651,
'M4x10 Cap Screw:3');
#225=NEXT_ASSEMBLY_USAGE_OCCURRENCE('Table plate:1','Table plate:1',
'Table plate:1',#14652,#14653,'Table plate:1');
#226=NEXT_ASSEMBLY_USAGE_OCCURRENCE('Bent scale pointer:1',
'Bent scale pointer:1','Bent scale pointer:1',#14652,#14654,
'Bent scale pointer:1');
#227=NEXT_ASSEMBLY_USAGE_OCCURRENCE('Manual grip:1','Manual grip:1',
'Manual grip:1',#14652,#14655,'Manual grip:1');
#228=NEXT_ASSEMBLY_USAGE_OCCURRENCE(
'Flanged Linear Guide Carriage - 15 mm:2',
'Flanged Linear Guide Carriage - 15 mm:2',
'Flanged Linear Guide Carriage - 15 mm:2',#14652,#14656,
'Flanged Linear Guide Carriage - 15 mm:2');
#229=NEXT_ASSEMBLY_USAGE_OCCURRENCE('Flat Washer - M5:6',
'Flat Washer - M5:6','Flat Washer - M5:6',#14652,#14660,
'Flat Washer - M5:6');
#230=NEXT_ASSEMBLY_USAGE_OCCURRENCE('Cap Screw - M5x20:2',
'Cap Screw - M5x20:2','Cap Screw - M5x20:2',#14652,#14661,
'Cap Screw - M5x20:2');
#231=NEXT_ASSEMBLY_USAGE_OCCURRENCE('Flat Washer - M5:7',
'Flat Washer - M5:7','Flat Washer - M5:7',#14652,#14660,
'Flat Washer - M5:7');
#232=NEXT_ASSEMBLY_USAGE_OCCURRENCE('Cap Screw - M5x20:3',
'Cap Screw - M5x20:3','Cap Screw - M5x20:3',#14652,#14661,
'Cap Screw - M5x20:3');
#233=NEXT_ASSEMBLY_USAGE_OCCURRENCE('Flat Washer - M5:8',
'Flat Washer - M5:8','Flat Washer - M5:8',#14652,#14660,
'Flat Washer - M5:8');
#234=NEXT_ASSEMBLY_USAGE_OCCURRENCE('Cap Screw - M5x20:4',
'Cap Screw - M5x20:4','Cap Screw - M5x20:4',#14652,#14661,
'Cap Screw - M5x20:4');
#235=NEXT_ASSEMBLY_USAGE_OCCURRENCE('Flat Washer - M5:9',
'Flat Washer - M5:9','Flat Washer - M5:9',#14652,#14660,
'Flat Washer - M5:9');
#236=NEXT_ASSEMBLY_USAGE_OCCURRENCE('Cap Screw - M5x20:5',
'Cap Screw - M5x20:5','Cap Screw - M5x20:5',#14652,#14661,
'Cap Screw - M5x20:5');
#237=NEXT_ASSEMBLY_USAGE_OCCURRENCE('Flat Washer - M4:4',
'Flat Washer - M4:4','Flat Washer - M4:4',#14652,#14662,
'Flat Washer - M4:4');
#238=NEXT_ASSEMBLY_USAGE_OCCURRENCE('Cap Screw - M4x16:6',
'Cap Screw - M4x16:6','Cap Screw - M4x16:6',#14652,#14663,
'Cap Screw - M4x16:6');
#239=NEXT_ASSEMBLY_USAGE_OCCURRENCE('Flat Washer - M6:2',
'Flat Washer - M6:2','Flat Washer - M6:2',#14652,#14664,
'Flat Washer - M6:2');
#240=NEXT_ASSEMBLY_USAGE_OCCURRENCE('Cap Screw - M6x25:2',
'Cap Screw - M6x25:2','Cap Screw - M6x25:2',#14652,#14665,
'Cap Screw - M6x25:2');
#241=NEXT_ASSEMBLY_USAGE_OCCURRENCE('Stationary frame:1',
'Stationary frame:1','Stationary frame:1',#14635,#14636,
'Stationary frame:1');
#242=NEXT_ASSEMBLY_USAGE_OCCURRENCE('Moving table:1','Moving table:1',
'Moving table:1',#14635,#14652,'Moving table:1');
#243=CONICAL_SURFACE('',#9310,0.4,0.785398163397448);
#244=CONICAL_SURFACE('',#9314,0.41,0.785398163397448);
#245=CONICAL_SURFACE('',#9318,0.26,0.463647609000806);
#246=CONICAL_SURFACE('',#9334,0.325,0.785398163397448);
#247=CONICAL_SURFACE('',#9338,0.335,0.785398163397448);
#248=CONICAL_SURFACE('',#9342,0.21,0.463647609000806);
#249=CONICAL_SURFACE('',#9458,0.275,0.785398163397449);
#250=CONICAL_SURFACE('',#9471,0.4,0.785398163397448);
#251=CONICAL_SURFACE('',#9475,0.41,0.785398163397448);
#252=CONICAL_SURFACE('',#9479,0.26,0.463647609000806);
#253=CONICAL_SURFACE('',#9483,0.225,0.785398163397448);
#254=CONICAL_SURFACE('',#9495,0.225,0.785398163397448);
#255=CONICAL_SURFACE('',#9508,0.325,0.785398163397448);
#256=CONICAL_SURFACE('',#9512,0.335,0.785398163397448);
#257=CONICAL_SURFACE('',#9516,0.21,0.463647609000806);
#258=CONICAL_SURFACE('',#9520,0.18,0.785398163397448);
#259=CONICAL_SURFACE('',#9580,0.475,0.785398163397449);
#260=CONICAL_SURFACE('',#9584,0.485,0.785398163397448);
#261=CONICAL_SURFACE('',#9588,0.31,0.463647609000806);
#262=CONICAL_SURFACE('',#9592,0.27,0.785398163397448);
#263=ORIENTED_CLOSED_SHELL('',*,#8602,.F.);
#264=ORIENTED_CLOSED_SHELL('',*,#8604,.F.);
#265=ORIENTED_CLOSED_SHELL('',*,#8614,.F.);
#266=ORIENTED_CLOSED_SHELL('',*,#8617,.F.);
#267=ORIENTED_CLOSED_SHELL('',*,#8620,.F.);
#268=BREP_WITH_VOIDS('Body1',#8603,(#263));
#269=BREP_WITH_VOIDS('Body1',#8605,(#264));
#270=BREP_WITH_VOIDS('Body1',#8613,(#265));
#271=BREP_WITH_VOIDS('Body1',#8616,(#266));
#272=BREP_WITH_VOIDS('Body1',#8619,(#267));
#273=ELLIPSE('',#9287,0.299389011154384,0.2117);
#274=ELLIPSE('',#9291,0.299389011154384,0.2117);
#275=SHAPE_REPRESENTATION_RELATIONSHIP('SRR','None',#14605,#302);
#276=SHAPE_REPRESENTATION_RELATIONSHIP('SRR','None',#14606,#303);
#277=SHAPE_REPRESENTATION_RELATIONSHIP('SRR','None',#14607,#304);
#278=SHAPE_REPRESENTATION_RELATIONSHIP('SRR','None',#14608,#305);
#279=SHAPE_REPRESENTATION_RELATIONSHIP('SRR','None',#14609,#306);
#280=SHAPE_REPRESENTATION_RELATIONSHIP('SRR','None',#14610,#307);
#281=SHAPE_REPRESENTATION_RELATIONSHIP('SRR','None',#14611,#308);
#282=SHAPE_REPRESENTATION_RELATIONSHIP('SRR','None',#14612,#309);
#283=SHAPE_REPRESENTATION_RELATIONSHIP('SRR','None',#14613,#310);
#284=SHAPE_REPRESENTATION_RELATIONSHIP('SRR','None',#14614,#311);
#285=SHAPE_REPRESENTATION_RELATIONSHIP('SRR','None',#14615,#312);
#286=SHAPE_REPRESENTATION_RELATIONSHIP('SRR','None',#14616,#313);
#287=SHAPE_REPRESENTATION_RELATIONSHIP('SRR','None',#14617,#314);
#288=SHAPE_REPRESENTATION_RELATIONSHIP('SRR','None',#14618,#315);
#289=SHAPE_REPRESENTATION_RELATIONSHIP('SRR','None',#14619,#316);
#290=SHAPE_REPRESENTATION_RELATIONSHIP('SRR','None',#14621,#317);
#291=SHAPE_REPRESENTATION_RELATIONSHIP('SRR','None',#14622,#318);
#292=SHAPE_REPRESENTATION_RELATIONSHIP('SRR','None',#14623,#319);
#293=SHAPE_REPRESENTATION_RELATIONSHIP('SRR','None',#14625,#320);
#294=SHAPE_REPRESENTATION_RELATIONSHIP('SRR','None',#14626,#321);
#295=SHAPE_REPRESENTATION_RELATIONSHIP('SRR','None',#14627,#322);
#296=SHAPE_REPRESENTATION_RELATIONSHIP('SRR','None',#14628,#323);
#297=SHAPE_REPRESENTATION_RELATIONSHIP('SRR','None',#14629,#324);
#298=SHAPE_REPRESENTATION_RELATIONSHIP('SRR','None',#14630,#325);
#299=SHAPE_REPRESENTATION_RELATIONSHIP('SRR','None',#14631,#326);
#300=SHAPE_REPRESENTATION_RELATIONSHIP('SRR','None',#14632,#327);
#301=SHAPE_REPRESENTATION_RELATIONSHIP('SRR','None',#14633,#328);
#302=ADVANCED_BREP_SHAPE_REPRESENTATION('',(#356),#14449);
#303=ADVANCED_BREP_SHAPE_REPRESENTATION('',(#357),#14450);
#304=ADVANCED_BREP_SHAPE_REPRESENTATION('',(#358),#14451);
#305=ADVANCED_BREP_SHAPE_REPRESENTATION('',(#359),#14452);
#306=ADVANCED_BREP_SHAPE_REPRESENTATION('',(#360),#14453);
#307=ADVANCED_BREP_SHAPE_REPRESENTATION('',(#361),#14454);
#308=ADVANCED_BREP_SHAPE_REPRESENTATION('',(#362),#14455);
#309=ADVANCED_BREP_SHAPE_REPRESENTATION('',(#363),#14456);
#310=ADVANCED_BREP_SHAPE_REPRESENTATION('',(#364),#14457);
#311=ADVANCED_BREP_SHAPE_REPRESENTATION('',(#365),#14458);
#312=ADVANCED_BREP_SHAPE_REPRESENTATION('',(#366),#14459);
#313=ADVANCED_BREP_SHAPE_REPRESENTATION('',(#367),#14460);
#314=ADVANCED_BREP_SHAPE_REPRESENTATION('',(#368),#14461);
#315=ADVANCED_BREP_SHAPE_REPRESENTATION('',(#268),#14462);
#316=ADVANCED_BREP_SHAPE_REPRESENTATION('',(#269),#14463);
#317=ADVANCED_BREP_SHAPE_REPRESENTATION('',(#369),#14465);
#318=ADVANCED_BREP_SHAPE_REPRESENTATION('',(#370),#14466);
#319=ADVANCED_BREP_SHAPE_REPRESENTATION('',(#371),#14467);
#320=ADVANCED_BREP_SHAPE_REPRESENTATION('',(#372),#14469);
#321=ADVANCED_BREP_SHAPE_REPRESENTATION('',(#373),#14470);
#322=ADVANCED_BREP_SHAPE_REPRESENTATION('',(#374),#14471);
#323=ADVANCED_BREP_SHAPE_REPRESENTATION('',(#375),#14472);
#324=ADVANCED_BREP_SHAPE_REPRESENTATION('',(#270),#14473);
#325=ADVANCED_BREP_SHAPE_REPRESENTATION('',(#376),#14474);
#326=ADVANCED_BREP_SHAPE_REPRESENTATION('',(#271),#14475);
#327=ADVANCED_BREP_SHAPE_REPRESENTATION('',(#377),#14476);
#328=ADVANCED_BREP_SHAPE_REPRESENTATION('',(#272),#14477);
#329=STYLED_ITEM('',(#14810),#356);
#330=STYLED_ITEM('',(#14824),#357);
#331=STYLED_ITEM('',(#14845),#358);
#332=STYLED_ITEM('',(#14824),#359);
#333=STYLED_ITEM('',(#14845),#360);
#334=STYLED_ITEM('',(#14845),#361);
#335=STYLED_ITEM('',(#14824),#362);
#336=STYLED_ITEM('',(#14824),#363);
#337=STYLED_ITEM('',(#14824),#364);
#338=STYLED_ITEM('',(#14824),#365);
#339=STYLED_ITEM('',(#14824),#366);
#340=STYLED_ITEM('',(#14845),#367);
#341=STYLED_ITEM('',(#14838),#368);
#342=STYLED_ITEM('',(#14838),#268);
#343=STYLED_ITEM('',(#14838),#269);
#344=STYLED_ITEM('',(#14824),#369);
#345=STYLED_ITEM('',(#14845),#370);
#346=STYLED_ITEM('',(#14838),#371);
#347=STYLED_ITEM('',(#14810),#372);
#348=STYLED_ITEM('',(#14824),#373);
#349=STYLED_ITEM('',(#14845),#374);
#350=STYLED_ITEM('',(#14838),#375);
#351=STYLED_ITEM('',(#14838),#270);
#352=STYLED_ITEM('',(#14838),#376);
#353=STYLED_ITEM('',(#14838),#271);
#354=STYLED_ITEM('',(#14838),#377);
#355=STYLED_ITEM('',(#14838),#272);
#356=MANIFOLD_SOLID_BREP('Body1',#8589);
#357=MANIFOLD_SOLID_BREP('Body1',#8590);
#358=MANIFOLD_SOLID_BREP('Body1',#8591);
#359=MANIFOLD_SOLID_BREP('Body1',#8592);
#360=MANIFOLD_SOLID_BREP('Body1',#8593);
#361=MANIFOLD_SOLID_BREP('Body1',#8594);
#362=MANIFOLD_SOLID_BREP('Body1',#8595);
#363=MANIFOLD_SOLID_BREP('Body1',#8596);
#364=MANIFOLD_SOLID_BREP('Body1',#8597);
#365=MANIFOLD_SOLID_BREP('Body1',#8598);
#366=MANIFOLD_SOLID_BREP('Body1',#8599);
#367=MANIFOLD_SOLID_BREP('Body1',#8600);
#368=MANIFOLD_SOLID_BREP('Body1',#8601);
#369=MANIFOLD_SOLID_BREP('Body1',#8606);
#370=MANIFOLD_SOLID_BREP('Body1',#8607);
#371=MANIFOLD_SOLID_BREP('Body1',#8608);
#372=MANIFOLD_SOLID_BREP('Body1',#8609);
#373=MANIFOLD_SOLID_BREP('Body1',#8610);
#374=MANIFOLD_SOLID_BREP('Body1',#8611);
#375=MANIFOLD_SOLID_BREP('Body1',#8612);
#376=MANIFOLD_SOLID_BREP('Body1',#8615);
#377=MANIFOLD_SOLID_BREP('Body1',#8618);
#378=FACE_BOUND('',#1314,.T.);
#379=FACE_BOUND('',#1315,.T.);
#380=FACE_BOUND('',#1316,.T.);
#381=FACE_BOUND('',#1317,.T.);
#382=FACE_BOUND('',#1318,.T.);
#383=FACE_BOUND('',#1319,.T.);
#384=FACE_BOUND('',#1320,.T.);
#385=FACE_BOUND('',#1321,.T.);
#386=FACE_BOUND('',#1322,.T.);
#387=FACE_BOUND('',#1323,.T.);
#388=FACE_BOUND('',#1324,.T.);
#389=FACE_BOUND('',#1325,.T.);
#390=FACE_BOUND('',#1326,.T.);
#391=FACE_BOUND('',#1327,.T.);
#392=FACE_BOUND('',#1329,.T.);
#393=FACE_BOUND('',#1330,.T.);
#394=FACE_BOUND('',#1331,.T.);
#395=FACE_BOUND('',#1332,.T.);
#396=FACE_BOUND('',#1333,.T.);
#397=FACE_BOUND('',#1334,.T.);
#398=FACE_BOUND('',#1335,.T.);
#399=FACE_BOUND('',#1336,.T.);
#400=FACE_BOUND('',#1337,.T.);
#401=FACE_BOUND('',#1338,.T.);
#402=FACE_BOUND('',#1339,.T.);
#403=FACE_BOUND('',#1340,.T.);
#404=FACE_BOUND('',#1341,.T.);
#405=FACE_BOUND('',#1342,.T.);
#406=FACE_BOUND('',#1345,.T.);
#407=FACE_BOUND('',#1348,.T.);
#408=FACE_BOUND('',#1356,.T.);
#409=FACE_BOUND('',#1357,.T.);
#410=FACE_BOUND('',#1359,.T.);
#411=FACE_BOUND('',#1360,.T.);
#412=FACE_BOUND('',#1369,.T.);
#413=FACE_BOUND('',#1372,.T.);
#414=FACE_BOUND('',#1380,.T.);
#415=FACE_BOUND('',#1381,.T.);
#416=FACE_BOUND('',#1383,.T.);
#417=FACE_BOUND('',#1384,.T.);
#418=FACE_BOUND('',#1508,.T.);
#419=FACE_BOUND('',#1509,.T.);
#420=FACE_BOUND('',#1517,.T.);
#421=FACE_BOUND('',#1518,.T.);
#422=FACE_BOUND('',#1545,.T.);
#423=FACE_BOUND('',#1548,.T.);
#424=FACE_BOUND('',#1551,.T.);
#425=FACE_BOUND('',#1554,.T.);
#426=FACE_BOUND('',#1564,.T.);
#427=FACE_BOUND('',#1565,.T.);
#428=FACE_BOUND('',#1566,.T.);
#429=FACE_BOUND('',#1567,.T.);
#430=FACE_BOUND('',#1574,.T.);
#431=FACE_BOUND('',#1575,.T.);
#432=FACE_BOUND('',#1576,.T.);
#433=FACE_BOUND('',#1577,.T.);
#434=FACE_BOUND('',#1627,.T.);
#435=FACE_BOUND('',#1629,.T.);
#436=FACE_BOUND('',#1633,.T.);
#437=FACE_BOUND('',#1659,.T.);
#438=FACE_BOUND('',#1676,.T.);
#439=FACE_BOUND('',#1690,.T.);
#440=FACE_BOUND('',#1691,.T.);
#441=FACE_BOUND('',#1692,.T.);
#442=FACE_BOUND('',#1693,.T.);
#443=FACE_BOUND('',#1694,.T.);
#444=FACE_BOUND('',#1695,.T.);
#445=FACE_BOUND('',#1697,.T.);
#446=FACE_BOUND('',#1698,.T.);
#447=FACE_BOUND('',#1699,.T.);
#448=FACE_BOUND('',#1700,.T.);
#449=FACE_BOUND('',#1701,.T.);
#450=FACE_BOUND('',#1702,.T.);
#451=FACE_BOUND('',#1705,.T.);
#452=FACE_BOUND('',#1710,.T.);
#453=FACE_BOUND('',#1717,.T.);
#454=FACE_BOUND('',#1719,.T.);
#455=FACE_BOUND('',#1734,.T.);
#456=FACE_BOUND('',#1735,.T.);
#457=FACE_BOUND('',#1736,.T.);
#458=FACE_BOUND('',#1737,.T.);
#459=FACE_BOUND('',#1769,.T.);
#460=FACE_BOUND('',#1772,.T.);
#461=FACE_BOUND('',#1778,.T.);
#462=FACE_BOUND('',#1794,.T.);
#463=FACE_BOUND('',#1797,.T.);
#464=FACE_BOUND('',#1803,.T.);
#465=FACE_BOUND('',#1819,.T.);
#466=FACE_BOUND('',#1821,.T.);
#467=FACE_BOUND('',#1827,.T.);
#468=PLANE('',#8964);
#469=PLANE('',#8965);
#470=PLANE('',#8966);
#471=PLANE('',#8967);
#472=PLANE('',#8968);
#473=PLANE('',#8969);
#474=PLANE('',#8974);
#475=PLANE('',#8979);
#476=PLANE('',#8985);
#477=PLANE('',#8986);
#478=PLANE('',#8987);
#479=PLANE('',#8988);
#480=PLANE('',#8989);
#481=PLANE('',#8990);
#482=PLANE('',#8992);
#483=PLANE('',#8993);
#484=PLANE('',#8994);
#485=PLANE('',#8995);
#486=PLANE('',#8996);
#487=PLANE('',#8997);
#488=PLANE('',#9002);
#489=PLANE('',#9007);
#490=PLANE('',#9013);
#491=PLANE('',#9014);
#492=PLANE('',#9015);
#493=PLANE('',#9016);
#494=PLANE('',#9017);
#495=PLANE('',#9018);
#496=PLANE('',#9020);
#497=PLANE('',#9021);
#498=PLANE('',#9022);
#499=PLANE('',#9023);
#500=PLANE('',#9024);
#501=PLANE('',#9025);
#502=PLANE('',#9027);
#503=PLANE('',#9028);
#504=PLANE('',#9029);
#505=PLANE('',#9030);
#506=PLANE('',#9031);
#507=PLANE('',#9032);
#508=PLANE('',#9033);
#509=PLANE('',#9034);
#510=PLANE('',#9035);
#511=PLANE('',#9036);
#512=PLANE('',#9037);
#513=PLANE('',#9038);
#514=PLANE('',#9039);
#515=PLANE('',#9040);
#516=PLANE('',#9041);
#517=PLANE('',#9042);
#518=PLANE('',#9043);
#519=PLANE('',#9044);
#520=PLANE('',#9045);
#521=PLANE('',#9046);
#522=PLANE('',#9047);
#523=PLANE('',#9048);
#524=PLANE('',#9049);
#525=PLANE('',#9050);
#526=PLANE('',#9051);
#527=PLANE('',#9052);
#528=PLANE('',#9053);
#529=PLANE('',#9054);
#530=PLANE('',#9055);
#531=PLANE('',#9056);
#532=PLANE('',#9057);
#533=PLANE('',#9058);
#534=PLANE('',#9059);
#535=PLANE('',#9060);
#536=PLANE('',#9061);
#537=PLANE('',#9062);
#538=PLANE('',#9063);
#539=PLANE('',#9064);
#540=PLANE('',#9065);
#541=PLANE('',#9066);
#542=PLANE('',#9067);
#543=PLANE('',#9068);
#544=PLANE('',#9069);
#545=PLANE('',#9070);
#546=PLANE('',#9071);
#547=PLANE('',#9072);
#548=PLANE('',#9073);
#549=PLANE('',#9074);
#550=PLANE('',#9075);
#551=PLANE('',#9076);
#552=PLANE('',#9077);
#553=PLANE('',#9078);
#554=PLANE('',#9079);
#555=PLANE('',#9080);
#556=PLANE('',#9081);
#557=PLANE('',#9082);
#558=PLANE('',#9083);
#559=PLANE('',#9084);
#560=PLANE('',#9085);
#561=PLANE('',#9086);
#562=PLANE('',#9087);
#563=PLANE('',#9088);
#564=PLANE('',#9089);
#565=PLANE('',#9090);
#566=PLANE('',#9091);
#567=PLANE('',#9092);
#568=PLANE('',#9093);
#569=PLANE('',#9094);
#570=PLANE('',#9095);
#571=PLANE('',#9096);
#572=PLANE('',#9097);
#573=PLANE('',#9098);
#574=PLANE('',#9099);
#575=PLANE('',#9100);
#576=PLANE('',#9101);
#577=PLANE('',#9102);
#578=PLANE('',#9103);
#579=PLANE('',#9104);
#580=PLANE('',#9105);
#581=PLANE('',#9106);
#582=PLANE('',#9107);
#583=PLANE('',#9108);
#584=PLANE('',#9109);
#585=PLANE('',#9110);
#586=PLANE('',#9111);
#587=PLANE('',#9112);
#588=PLANE('',#9113);
#589=PLANE('',#9114);
#590=PLANE('',#9115);
#591=PLANE('',#9116);
#592=PLANE('',#9117);
#593=PLANE('',#9118);
#594=PLANE('',#9119);
#595=PLANE('',#9120);
#596=PLANE('',#9121);
#597=PLANE('',#9122);
#598=PLANE('',#9123);
#599=PLANE('',#9124);
#600=PLANE('',#9125);
#601=PLANE('',#9126);
#602=PLANE('',#9127);
#603=PLANE('',#9128);
#604=PLANE('',#9129);
#605=PLANE('',#9130);
#606=PLANE('',#9131);
#607=PLANE('',#9132);
#608=PLANE('',#9133);
#609=PLANE('',#9134);
#610=PLANE('',#9135);
#611=PLANE('',#9136);
#612=PLANE('',#9137);
#613=PLANE('',#9138);
#614=PLANE('',#9139);
#615=PLANE('',#9140);
#616=PLANE('',#9141);
#617=PLANE('',#9142);
#618=PLANE('',#9143);
#619=PLANE('',#9150);
#620=PLANE('',#9151);
#621=PLANE('',#9152);
#622=PLANE('',#9153);
#623=PLANE('',#9154);
#624=PLANE('',#9156);
#625=PLANE('',#9157);
#626=PLANE('',#9158);
#627=PLANE('',#9159);
#628=PLANE('',#9160);
#629=PLANE('',#9161);
#630=PLANE('',#9163);
#631=PLANE('',#9164);
#632=PLANE('',#9165);
#633=PLANE('',#9166);
#634=PLANE('',#9167);
#635=PLANE('',#9168);
#636=PLANE('',#9170);
#637=PLANE('',#9171);
#638=PLANE('',#9172);
#639=PLANE('',#9173);
#640=PLANE('',#9174);
#641=PLANE('',#9175);
#642=PLANE('',#9177);
#643=PLANE('',#9178);
#644=PLANE('',#9179);
#645=PLANE('',#9180);
#646=PLANE('',#9181);
#647=PLANE('',#9182);
#648=PLANE('',#9187);
#649=PLANE('',#9192);
#650=PLANE('',#9197);
#651=PLANE('',#9202);
#652=PLANE('',#9212);
#653=PLANE('',#9213);
#654=PLANE('',#9214);
#655=PLANE('',#9215);
#656=PLANE('',#9216);
#657=PLANE('',#9217);
#658=PLANE('',#9218);
#659=PLANE('',#9219);
#660=PLANE('',#9220);
#661=PLANE('',#9221);
#662=PLANE('',#9222);
#663=PLANE('',#9223);
#664=PLANE('',#9224);
#665=PLANE('',#9225);
#666=PLANE('',#9227);
#667=PLANE('',#9228);
#668=PLANE('',#9229);
#669=PLANE('',#9230);
#670=PLANE('',#9231);
#671=PLANE('',#9232);
#672=PLANE('',#9233);
#673=PLANE('',#9234);
#674=PLANE('',#9235);
#675=PLANE('',#9236);
#676=PLANE('',#9237);
#677=PLANE('',#9238);
#678=PLANE('',#9239);
#679=PLANE('',#9240);
#680=PLANE('',#9241);
#681=PLANE('',#9242);
#682=PLANE('',#9243);
#683=PLANE('',#9244);
#684=PLANE('',#9245);
#685=PLANE('',#9246);
#686=PLANE('',#9247);
#687=PLANE('',#9248);
#688=PLANE('',#9249);
#689=PLANE('',#9250);
#690=PLANE('',#9251);
#691=PLANE('',#9252);
#692=PLANE('',#9253);
#693=PLANE('',#9254);
#694=PLANE('',#9255);
#695=PLANE('',#9256);
#696=PLANE('',#9257);
#697=PLANE('',#9258);
#698=PLANE('',#9259);
#699=PLANE('',#9260);
#700=PLANE('',#9261);
#701=PLANE('',#9262);
#702=PLANE('',#9266);
#703=PLANE('',#9267);
#704=PLANE('',#9268);
#705=PLANE('',#9269);
#706=PLANE('',#9270);
#707=PLANE('',#9271);
#708=PLANE('',#9272);
#709=PLANE('',#9273);
#710=PLANE('',#9274);
#711=PLANE('',#9275);
#712=PLANE('',#9277);
#713=PLANE('',#9278);
#714=PLANE('',#9279);
#715=PLANE('',#9281);
#716=PLANE('',#9282);
#717=PLANE('',#9283);
#718=PLANE('',#9284);
#719=PLANE('',#9285);
#720=PLANE('',#9286);
#721=PLANE('',#9293);
#722=PLANE('',#9294);
#723=PLANE('',#9295);
#724=PLANE('',#9296);
#725=PLANE('',#9298);
#726=PLANE('',#9299);
#727=PLANE('',#9300);
#728=PLANE('',#9301);
#729=PLANE('',#9302);
#730=PLANE('',#9303);
#731=PLANE('',#9304);
#732=PLANE('',#9305);
#733=PLANE('',#9306);
#734=PLANE('',#9308);
#735=PLANE('',#9316);
#736=PLANE('',#9322);
#737=PLANE('',#9323);
#738=PLANE('',#9324);
#739=PLANE('',#9325);
#740=PLANE('',#9326);
#741=PLANE('',#9327);
#742=PLANE('',#9328);
#743=PLANE('',#9329);
#744=PLANE('',#9330);
#745=PLANE('',#9332);
#746=PLANE('',#9340);
#747=PLANE('',#9365);
#748=PLANE('',#9366);
#749=PLANE('',#9367);
#750=PLANE('',#9368);
#751=PLANE('',#9369);
#752=PLANE('',#9370);
#753=PLANE('',#9375);
#754=PLANE('',#9376);
#755=PLANE('',#9377);
#756=PLANE('',#9378);
#757=PLANE('',#9379);
#758=PLANE('',#9380);
#759=PLANE('',#9381);
#760=PLANE('',#9382);
#761=PLANE('',#9390);
#762=PLANE('',#9391);
#763=PLANE('',#9394);
#764=PLANE('',#9400);
#765=PLANE('',#9406);
#766=PLANE('',#9412);
#767=PLANE('',#9418);
#768=PLANE('',#9419);
#769=PLANE('',#9420);
#770=PLANE('',#9421);
#771=PLANE('',#9422);
#772=PLANE('',#9423);
#773=PLANE('',#9424);
#774=PLANE('',#9425);
#775=PLANE('',#9426);
#776=PLANE('',#9427);
#777=PLANE('',#9428);
#778=PLANE('',#9429);
#779=PLANE('',#9430);
#780=PLANE('',#9431);
#781=PLANE('',#9433);
#782=PLANE('',#9434);
#783=PLANE('',#9435);
#784=PLANE('',#9436);
#785=PLANE('',#9437);
#786=PLANE('',#9438);
#787=PLANE('',#9439);
#788=PLANE('',#9440);
#789=PLANE('',#9441);
#790=PLANE('',#9442);
#791=PLANE('',#9444);
#792=PLANE('',#9445);
#793=PLANE('',#9446);
#794=PLANE('',#9447);
#795=PLANE('',#9448);
#796=PLANE('',#9449);
#797=PLANE('',#9450);
#798=PLANE('',#9451);
#799=PLANE('',#9452);
#800=PLANE('',#9453);
#801=PLANE('',#9463);
#802=PLANE('',#9467);
#803=PLANE('',#9469);
#804=PLANE('',#9477);
#805=PLANE('',#9485);
#806=PLANE('',#9486);
#807=PLANE('',#9487);
#808=PLANE('',#9488);
#809=PLANE('',#9489);
#810=PLANE('',#9490);
#811=PLANE('',#9491);
#812=PLANE('',#9492);
#813=PLANE('',#9493);
#814=PLANE('',#9500);
#815=PLANE('',#9504);
#816=PLANE('',#9506);
#817=PLANE('',#9514);
#818=PLANE('',#9522);
#819=PLANE('',#9523);
#820=PLANE('',#9524);
#821=PLANE('',#9525);
#822=PLANE('',#9526);
#823=PLANE('',#9527);
#824=PLANE('',#9528);
#825=PLANE('',#9529);
#826=PLANE('',#9530);
#827=PLANE('',#9575);
#828=PLANE('',#9576);
#829=PLANE('',#9578);
#830=PLANE('',#9586);
#831=PLANE('',#9594);
#832=PLANE('',#9595);
#833=PLANE('',#9596);
#834=PLANE('',#9597);
#835=PLANE('',#9598);
#836=PLANE('',#9599);
#837=PLANE('',#9600);
#838=PLANE('',#9601);
#839=PLANE('',#9602);
#840=FACE_OUTER_BOUND('',#1295,.T.);
#841=FACE_OUTER_BOUND('',#1296,.T.);
#842=FACE_OUTER_BOUND('',#1297,.T.);
#843=FACE_OUTER_BOUND('',#1298,.T.);
#844=FACE_OUTER_BOUND('',#1299,.T.);
#845=FACE_OUTER_BOUND('',#1300,.T.);
#846=FACE_OUTER_BOUND('',#1301,.T.);
#847=FACE_OUTER_BOUND('',#1302,.T.);
#848=FACE_OUTER_BOUND('',#1303,.T.);
#849=FACE_OUTER_BOUND('',#1304,.T.);
#850=FACE_OUTER_BOUND('',#1305,.T.);
#851=FACE_OUTER_BOUND('',#1306,.T.);
#852=FACE_OUTER_BOUND('',#1307,.T.);
#853=FACE_OUTER_BOUND('',#1308,.T.);
#854=FACE_OUTER_BOUND('',#1309,.T.);
#855=FACE_OUTER_BOUND('',#1310,.T.);
#856=FACE_OUTER_BOUND('',#1311,.T.);
#857=FACE_OUTER_BOUND('',#1312,.T.);
#858=FACE_OUTER_BOUND('',#1313,.T.);
#859=FACE_OUTER_BOUND('',#1328,.T.);
#860=FACE_OUTER_BOUND('',#1343,.T.);
#861=FACE_OUTER_BOUND('',#1344,.T.);
#862=FACE_OUTER_BOUND('',#1346,.T.);
#863=FACE_OUTER_BOUND('',#1347,.T.);
#864=FACE_OUTER_BOUND('',#1349,.T.);
#865=FACE_OUTER_BOUND('',#1350,.T.);
#866=FACE_OUTER_BOUND('',#1351,.T.);
#867=FACE_OUTER_BOUND('',#1352,.T.);
#868=FACE_OUTER_BOUND('',#1353,.T.);
#869=FACE_OUTER_BOUND('',#1354,.T.);
#870=FACE_OUTER_BOUND('',#1355,.T.);
#871=FACE_OUTER_BOUND('',#1358,.T.);
#872=FACE_OUTER_BOUND('',#1361,.T.);
#873=FACE_OUTER_BOUND('',#1362,.T.);
#874=FACE_OUTER_BOUND('',#1363,.T.);
#875=FACE_OUTER_BOUND('',#1364,.T.);
#876=FACE_OUTER_BOUND('',#1365,.T.);
#877=FACE_OUTER_BOUND('',#1366,.T.);
#878=FACE_OUTER_BOUND('',#1367,.T.);
#879=FACE_OUTER_BOUND('',#1368,.T.);
#880=FACE_OUTER_BOUND('',#1370,.T.);
#881=FACE_OUTER_BOUND('',#1371,.T.);
#882=FACE_OUTER_BOUND('',#1373,.T.);
#883=FACE_OUTER_BOUND('',#1374,.T.);
#884=FACE_OUTER_BOUND('',#1375,.T.);
#885=FACE_OUTER_BOUND('',#1376,.T.);
#886=FACE_OUTER_BOUND('',#1377,.T.);
#887=FACE_OUTER_BOUND('',#1378,.T.);
#888=FACE_OUTER_BOUND('',#1379,.T.);
#889=FACE_OUTER_BOUND('',#1382,.T.);
#890=FACE_OUTER_BOUND('',#1385,.T.);
#891=FACE_OUTER_BOUND('',#1386,.T.);
#892=FACE_OUTER_BOUND('',#1387,.T.);
#893=FACE_OUTER_BOUND('',#1388,.T.);
#894=FACE_OUTER_BOUND('',#1389,.T.);
#895=FACE_OUTER_BOUND('',#1390,.T.);
#896=FACE_OUTER_BOUND('',#1391,.T.);
#897=FACE_OUTER_BOUND('',#1392,.T.);
#898=FACE_OUTER_BOUND('',#1393,.T.);
#899=FACE_OUTER_BOUND('',#1394,.T.);
#900=FACE_OUTER_BOUND('',#1395,.T.);
#901=FACE_OUTER_BOUND('',#1396,.T.);
#902=FACE_OUTER_BOUND('',#1397,.T.);
#903=FACE_OUTER_BOUND('',#1398,.T.);
#904=FACE_OUTER_BOUND('',#1399,.T.);
#905=FACE_OUTER_BOUND('',#1400,.T.);
#906=FACE_OUTER_BOUND('',#1401,.T.);
#907=FACE_OUTER_BOUND('',#1402,.T.);
#908=FACE_OUTER_BOUND('',#1403,.T.);
#909=FACE_OUTER_BOUND('',#1404,.T.);
#910=FACE_OUTER_BOUND('',#1405,.T.);
#911=FACE_OUTER_BOUND('',#1406,.T.);
#912=FACE_OUTER_BOUND('',#1407,.T.);
#913=FACE_OUTER_BOUND('',#1408,.T.);
#914=FACE_OUTER_BOUND('',#1409,.T.);
#915=FACE_OUTER_BOUND('',#1410,.T.);
#916=FACE_OUTER_BOUND('',#1411,.T.);
#917=FACE_OUTER_BOUND('',#1412,.T.);
#918=FACE_OUTER_BOUND('',#1413,.T.);
#919=FACE_OUTER_BOUND('',#1414,.T.);
#920=FACE_OUTER_BOUND('',#1415,.T.);
#921=FACE_OUTER_BOUND('',#1416,.T.);
#922=FACE_OUTER_BOUND('',#1417,.T.);
#923=FACE_OUTER_BOUND('',#1418,.T.);
#924=FACE_OUTER_BOUND('',#1419,.T.);
#925=FACE_OUTER_BOUND('',#1420,.T.);
#926=FACE_OUTER_BOUND('',#1421,.T.);
#927=FACE_OUTER_BOUND('',#1422,.T.);
#928=FACE_OUTER_BOUND('',#1423,.T.);
#929=FACE_OUTER_BOUND('',#1424,.T.);
#930=FACE_OUTER_BOUND('',#1425,.T.);
#931=FACE_OUTER_BOUND('',#1426,.T.);
#932=FACE_OUTER_BOUND('',#1427,.T.);
#933=FACE_OUTER_BOUND('',#1428,.T.);
#934=FACE_OUTER_BOUND('',#1429,.T.);
#935=FACE_OUTER_BOUND('',#1430,.T.);
#936=FACE_OUTER_BOUND('',#1431,.T.);
#937=FACE_OUTER_BOUND('',#1432,.T.);
#938=FACE_OUTER_BOUND('',#1433,.T.);
#939=FACE_OUTER_BOUND('',#1434,.T.);
#940=FACE_OUTER_BOUND('',#1435,.T.);
#941=FACE_OUTER_BOUND('',#1436,.T.);
#942=FACE_OUTER_BOUND('',#1437,.T.);
#943=FACE_OUTER_BOUND('',#1438,.T.);
#944=FACE_OUTER_BOUND('',#1439,.T.);
#945=FACE_OUTER_BOUND('',#1440,.T.);
#946=FACE_OUTER_BOUND('',#1441,.T.);
#947=FACE_OUTER_BOUND('',#1442,.T.);
#948=FACE_OUTER_BOUND('',#1443,.T.);
#949=FACE_OUTER_BOUND('',#1444,.T.);
#950=FACE_OUTER_BOUND('',#1445,.T.);
#951=FACE_OUTER_BOUND('',#1446,.T.);
#952=FACE_OUTER_BOUND('',#1447,.T.);
#953=FACE_OUTER_BOUND('',#1448,.T.);
#954=FACE_OUTER_BOUND('',#1449,.T.);
#955=FACE_OUTER_BOUND('',#1450,.T.);
#956=FACE_OUTER_BOUND('',#1451,.T.);
#957=FACE_OUTER_BOUND('',#1452,.T.);
#958=FACE_OUTER_BOUND('',#1453,.T.);
#959=FACE_OUTER_BOUND('',#1454,.T.);
#960=FACE_OUTER_BOUND('',#1455,.T.);
#961=FACE_OUTER_BOUND('',#1456,.T.);
#962=FACE_OUTER_BOUND('',#1457,.T.);
#963=FACE_OUTER_BOUND('',#1458,.T.);
#964=FACE_OUTER_BOUND('',#1459,.T.);
#965=FACE_OUTER_BOUND('',#1460,.T.);
#966=FACE_OUTER_BOUND('',#1461,.T.);
#967=FACE_OUTER_BOUND('',#1462,.T.);
#968=FACE_OUTER_BOUND('',#1463,.T.);
#969=FACE_OUTER_BOUND('',#1464,.T.);
#970=FACE_OUTER_BOUND('',#1465,.T.);
#971=FACE_OUTER_BOUND('',#1466,.T.);
#972=FACE_OUTER_BOUND('',#1467,.T.);
#973=FACE_OUTER_BOUND('',#1468,.T.);
#974=FACE_OUTER_BOUND('',#1469,.T.);
#975=FACE_OUTER_BOUND('',#1470,.T.);
#976=FACE_OUTER_BOUND('',#1471,.T.);
#977=FACE_OUTER_BOUND('',#1472,.T.);
#978=FACE_OUTER_BOUND('',#1473,.T.);
#979=FACE_OUTER_BOUND('',#1474,.T.);
#980=FACE_OUTER_BOUND('',#1475,.T.);
#981=FACE_OUTER_BOUND('',#1476,.T.);
#982=FACE_OUTER_BOUND('',#1477,.T.);
#983=FACE_OUTER_BOUND('',#1478,.T.);
#984=FACE_OUTER_BOUND('',#1479,.T.);
#985=FACE_OUTER_BOUND('',#1480,.T.);
#986=FACE_OUTER_BOUND('',#1481,.T.);
#987=FACE_OUTER_BOUND('',#1482,.T.);
#988=FACE_OUTER_BOUND('',#1483,.T.);
#989=FACE_OUTER_BOUND('',#1484,.T.);
#990=FACE_OUTER_BOUND('',#1485,.T.);
#991=FACE_OUTER_BOUND('',#1486,.T.);
#992=FACE_OUTER_BOUND('',#1487,.T.);
#993=FACE_OUTER_BOUND('',#1488,.T.);
#994=FACE_OUTER_BOUND('',#1489,.T.);
#995=FACE_OUTER_BOUND('',#1490,.T.);
#996=FACE_OUTER_BOUND('',#1491,.T.);
#997=FACE_OUTER_BOUND('',#1492,.T.);
#998=FACE_OUTER_BOUND('',#1493,.T.);
#999=FACE_OUTER_BOUND('',#1494,.T.);
#1000=FACE_OUTER_BOUND('',#1495,.T.);
#1001=FACE_OUTER_BOUND('',#1496,.T.);
#1002=FACE_OUTER_BOUND('',#1497,.T.);
#1003=FACE_OUTER_BOUND('',#1498,.T.);
#1004=FACE_OUTER_BOUND('',#1499,.T.);
#1005=FACE_OUTER_BOUND('',#1500,.T.);
#1006=FACE_OUTER_BOUND('',#1501,.T.);
#1007=FACE_OUTER_BOUND('',#1502,.T.);
#1008=FACE_OUTER_BOUND('',#1503,.T.);
#1009=FACE_OUTER_BOUND('',#1504,.T.);
#1010=FACE_OUTER_BOUND('',#1505,.T.);
#1011=FACE_OUTER_BOUND('',#1506,.T.);
#1012=FACE_OUTER_BOUND('',#1507,.T.);
#1013=FACE_OUTER_BOUND('',#1510,.T.);
#1014=FACE_OUTER_BOUND('',#1511,.T.);
#1015=FACE_OUTER_BOUND('',#1512,.T.);
#1016=FACE_OUTER_BOUND('',#1513,.T.);
#1017=FACE_OUTER_BOUND('',#1514,.T.);
#1018=FACE_OUTER_BOUND('',#1515,.T.);
#1019=FACE_OUTER_BOUND('',#1516,.T.);
#1020=FACE_OUTER_BOUND('',#1519,.T.);
#1021=FACE_OUTER_BOUND('',#1520,.T.);
#1022=FACE_OUTER_BOUND('',#1521,.T.);
#1023=FACE_OUTER_BOUND('',#1522,.T.);
#1024=FACE_OUTER_BOUND('',#1523,.T.);
#1025=FACE_OUTER_BOUND('',#1524,.T.);
#1026=FACE_OUTER_BOUND('',#1525,.T.);
#1027=FACE_OUTER_BOUND('',#1526,.T.);
#1028=FACE_OUTER_BOUND('',#1527,.T.);
#1029=FACE_OUTER_BOUND('',#1528,.T.);
#1030=FACE_OUTER_BOUND('',#1529,.T.);
#1031=FACE_OUTER_BOUND('',#1530,.T.);
#1032=FACE_OUTER_BOUND('',#1531,.T.);
#1033=FACE_OUTER_BOUND('',#1532,.T.);
#1034=FACE_OUTER_BOUND('',#1533,.T.);
#1035=FACE_OUTER_BOUND('',#1534,.T.);
#1036=FACE_OUTER_BOUND('',#1535,.T.);
#1037=FACE_OUTER_BOUND('',#1536,.T.);
#1038=FACE_OUTER_BOUND('',#1537,.T.);
#1039=FACE_OUTER_BOUND('',#1538,.T.);
#1040=FACE_OUTER_BOUND('',#1539,.T.);
#1041=FACE_OUTER_BOUND('',#1540,.T.);
#1042=FACE_OUTER_BOUND('',#1541,.T.);
#1043=FACE_OUTER_BOUND('',#1542,.T.);
#1044=FACE_OUTER_BOUND('',#1543,.T.);
#1045=FACE_OUTER_BOUND('',#1544,.T.);
#1046=FACE_OUTER_BOUND('',#1546,.T.);
#1047=FACE_OUTER_BOUND('',#1547,.T.);
#1048=FACE_OUTER_BOUND('',#1549,.T.);
#1049=FACE_OUTER_BOUND('',#1550,.T.);
#1050=FACE_OUTER_BOUND('',#1552,.T.);
#1051=FACE_OUTER_BOUND('',#1553,.T.);
#1052=FACE_OUTER_BOUND('',#1555,.T.);
#1053=FACE_OUTER_BOUND('',#1556,.T.);
#1054=FACE_OUTER_BOUND('',#1557,.T.);
#1055=FACE_OUTER_BOUND('',#1558,.T.);
#1056=FACE_OUTER_BOUND('',#1559,.T.);
#1057=FACE_OUTER_BOUND('',#1560,.T.);
#1058=FACE_OUTER_BOUND('',#1561,.T.);
#1059=FACE_OUTER_BOUND('',#1562,.T.);
#1060=FACE_OUTER_BOUND('',#1563,.T.);
#1061=FACE_OUTER_BOUND('',#1568,.T.);
#1062=FACE_OUTER_BOUND('',#1569,.T.);
#1063=FACE_OUTER_BOUND('',#1570,.T.);
#1064=FACE_OUTER_BOUND('',#1571,.T.);
#1065=FACE_OUTER_BOUND('',#1572,.T.);
#1066=FACE_OUTER_BOUND('',#1573,.T.);
#1067=FACE_OUTER_BOUND('',#1578,.T.);
#1068=FACE_OUTER_BOUND('',#1579,.T.);
#1069=FACE_OUTER_BOUND('',#1580,.T.);
#1070=FACE_OUTER_BOUND('',#1581,.T.);
#1071=FACE_OUTER_BOUND('',#1582,.T.);
#1072=FACE_OUTER_BOUND('',#1583,.T.);
#1073=FACE_OUTER_BOUND('',#1584,.T.);
#1074=FACE_OUTER_BOUND('',#1585,.T.);
#1075=FACE_OUTER_BOUND('',#1586,.T.);
#1076=FACE_OUTER_BOUND('',#1587,.T.);
#1077=FACE_OUTER_BOUND('',#1588,.T.);
#1078=FACE_OUTER_BOUND('',#1589,.T.);
#1079=FACE_OUTER_BOUND('',#1590,.T.);
#1080=FACE_OUTER_BOUND('',#1591,.T.);
#1081=FACE_OUTER_BOUND('',#1592,.T.);
#1082=FACE_OUTER_BOUND('',#1593,.T.);
#1083=FACE_OUTER_BOUND('',#1594,.T.);
#1084=FACE_OUTER_BOUND('',#1595,.T.);
#1085=FACE_OUTER_BOUND('',#1596,.T.);
#1086=FACE_OUTER_BOUND('',#1597,.T.);
#1087=FACE_OUTER_BOUND('',#1598,.T.);
#1088=FACE_OUTER_BOUND('',#1599,.T.);
#1089=FACE_OUTER_BOUND('',#1600,.T.);
#1090=FACE_OUTER_BOUND('',#1601,.T.);
#1091=FACE_OUTER_BOUND('',#1602,.T.);
#1092=FACE_OUTER_BOUND('',#1603,.T.);
#1093=FACE_OUTER_BOUND('',#1604,.T.);
#1094=FACE_OUTER_BOUND('',#1605,.T.);
#1095=FACE_OUTER_BOUND('',#1606,.T.);
#1096=FACE_OUTER_BOUND('',#1607,.T.);
#1097=FACE_OUTER_BOUND('',#1608,.T.);
#1098=FACE_OUTER_BOUND('',#1609,.T.);
#1099=FACE_OUTER_BOUND('',#1610,.T.);
#1100=FACE_OUTER_BOUND('',#1611,.T.);
#1101=FACE_OUTER_BOUND('',#1612,.T.);
#1102=FACE_OUTER_BOUND('',#1613,.T.);
#1103=FACE_OUTER_BOUND('',#1614,.T.);
#1104=FACE_OUTER_BOUND('',#1615,.T.);
#1105=FACE_OUTER_BOUND('',#1616,.T.);
#1106=FACE_OUTER_BOUND('',#1617,.T.);
#1107=FACE_OUTER_BOUND('',#1618,.T.);
#1108=FACE_OUTER_BOUND('',#1619,.T.);
#1109=FACE_OUTER_BOUND('',#1620,.T.);
#1110=FACE_OUTER_BOUND('',#1621,.T.);
#1111=FACE_OUTER_BOUND('',#1622,.T.);
#1112=FACE_OUTER_BOUND('',#1623,.T.);
#1113=FACE_OUTER_BOUND('',#1624,.T.);
#1114=FACE_OUTER_BOUND('',#1625,.T.);
#1115=FACE_OUTER_BOUND('',#1626,.T.);
#1116=FACE_OUTER_BOUND('',#1628,.T.);
#1117=FACE_OUTER_BOUND('',#1630,.T.);
#1118=FACE_OUTER_BOUND('',#1631,.T.);
#1119=FACE_OUTER_BOUND('',#1632,.T.);
#1120=FACE_OUTER_BOUND('',#1634,.T.);
#1121=FACE_OUTER_BOUND('',#1635,.T.);
#1122=FACE_OUTER_BOUND('',#1636,.T.);
#1123=FACE_OUTER_BOUND('',#1637,.T.);
#1124=FACE_OUTER_BOUND('',#1638,.T.);
#1125=FACE_OUTER_BOUND('',#1639,.T.);
#1126=FACE_OUTER_BOUND('',#1640,.T.);
#1127=FACE_OUTER_BOUND('',#1641,.T.);
#1128=FACE_OUTER_BOUND('',#1642,.T.);
#1129=FACE_OUTER_BOUND('',#1643,.T.);
#1130=FACE_OUTER_BOUND('',#1644,.T.);
#1131=FACE_OUTER_BOUND('',#1645,.T.);
#1132=FACE_OUTER_BOUND('',#1646,.T.);
#1133=FACE_OUTER_BOUND('',#1647,.T.);
#1134=FACE_OUTER_BOUND('',#1648,.T.);
#1135=FACE_OUTER_BOUND('',#1649,.T.);
#1136=FACE_OUTER_BOUND('',#1650,.T.);
#1137=FACE_OUTER_BOUND('',#1651,.T.);
#1138=FACE_OUTER_BOUND('',#1652,.T.);
#1139=FACE_OUTER_BOUND('',#1653,.T.);
#1140=FACE_OUTER_BOUND('',#1654,.T.);
#1141=FACE_OUTER_BOUND('',#1655,.T.);
#1142=FACE_OUTER_BOUND('',#1656,.T.);
#1143=FACE_OUTER_BOUND('',#1657,.T.);
#1144=FACE_OUTER_BOUND('',#1658,.T.);
#1145=FACE_OUTER_BOUND('',#1660,.T.);
#1146=FACE_OUTER_BOUND('',#1661,.T.);
#1147=FACE_OUTER_BOUND('',#1662,.T.);
#1148=FACE_OUTER_BOUND('',#1663,.T.);
#1149=FACE_OUTER_BOUND('',#1664,.T.);
#1150=FACE_OUTER_BOUND('',#1665,.T.);
#1151=FACE_OUTER_BOUND('',#1666,.T.);
#1152=FACE_OUTER_BOUND('',#1667,.T.);
#1153=FACE_OUTER_BOUND('',#1668,.T.);
#1154=FACE_OUTER_BOUND('',#1669,.T.);
#1155=FACE_OUTER_BOUND('',#1670,.T.);
#1156=FACE_OUTER_BOUND('',#1671,.T.);
#1157=FACE_OUTER_BOUND('',#1672,.T.);
#1158=FACE_OUTER_BOUND('',#1673,.T.);
#1159=FACE_OUTER_BOUND('',#1674,.T.);
#1160=FACE_OUTER_BOUND('',#1675,.T.);
#1161=FACE_OUTER_BOUND('',#1677,.T.);
#1162=FACE_OUTER_BOUND('',#1678,.T.);
#1163=FACE_OUTER_BOUND('',#1679,.T.);
#1164=FACE_OUTER_BOUND('',#1680,.T.);
#1165=FACE_OUTER_BOUND('',#1681,.T.);
#1166=FACE_OUTER_BOUND('',#1682,.T.);
#1167=FACE_OUTER_BOUND('',#1683,.T.);
#1168=FACE_OUTER_BOUND('',#1684,.T.);
#1169=FACE_OUTER_BOUND('',#1685,.T.);
#1170=FACE_OUTER_BOUND('',#1686,.T.);
#1171=FACE_OUTER_BOUND('',#1687,.T.);
#1172=FACE_OUTER_BOUND('',#1688,.T.);
#1173=FACE_OUTER_BOUND('',#1689,.T.);
#1174=FACE_OUTER_BOUND('',#1696,.T.);
#1175=FACE_OUTER_BOUND('',#1703,.T.);
#1176=FACE_OUTER_BOUND('',#1704,.T.);
#1177=FACE_OUTER_BOUND('',#1706,.T.);
#1178=FACE_OUTER_BOUND('',#1707,.T.);
#1179=FACE_OUTER_BOUND('',#1708,.T.);
#1180=FACE_OUTER_BOUND('',#1709,.T.);
#1181=FACE_OUTER_BOUND('',#1711,.T.);
#1182=FACE_OUTER_BOUND('',#1712,.T.);
#1183=FACE_OUTER_BOUND('',#1713,.T.);
#1184=FACE_OUTER_BOUND('',#1714,.T.);
#1185=FACE_OUTER_BOUND('',#1715,.T.);
#1186=FACE_OUTER_BOUND('',#1716,.T.);
#1187=FACE_OUTER_BOUND('',#1718,.T.);
#1188=FACE_OUTER_BOUND('',#1720,.T.);
#1189=FACE_OUTER_BOUND('',#1721,.T.);
#1190=FACE_OUTER_BOUND('',#1722,.T.);
#1191=FACE_OUTER_BOUND('',#1723,.T.);
#1192=FACE_OUTER_BOUND('',#1724,.T.);
#1193=FACE_OUTER_BOUND('',#1725,.T.);
#1194=FACE_OUTER_BOUND('',#1726,.T.);
#1195=FACE_OUTER_BOUND('',#1727,.T.);
#1196=FACE_OUTER_BOUND('',#1728,.T.);
#1197=FACE_OUTER_BOUND('',#1729,.T.);
#1198=FACE_OUTER_BOUND('',#1730,.T.);
#1199=FACE_OUTER_BOUND('',#1731,.T.);
#1200=FACE_OUTER_BOUND('',#1732,.T.);
#1201=FACE_OUTER_BOUND('',#1733,.T.);
#1202=FACE_OUTER_BOUND('',#1738,.T.);
#1203=FACE_OUTER_BOUND('',#1739,.T.);
#1204=FACE_OUTER_BOUND('',#1740,.T.);
#1205=FACE_OUTER_BOUND('',#1741,.T.);
#1206=FACE_OUTER_BOUND('',#1742,.T.);
#1207=FACE_OUTER_BOUND('',#1743,.T.);
#1208=FACE_OUTER_BOUND('',#1744,.T.);
#1209=FACE_OUTER_BOUND('',#1745,.T.);
#1210=FACE_OUTER_BOUND('',#1746,.T.);
#1211=FACE_OUTER_BOUND('',#1747,.T.);
#1212=FACE_OUTER_BOUND('',#1748,.T.);
#1213=FACE_OUTER_BOUND('',#1749,.T.);
#1214=FACE_OUTER_BOUND('',#1750,.T.);
#1215=FACE_OUTER_BOUND('',#1751,.T.);
#1216=FACE_OUTER_BOUND('',#1752,.T.);
#1217=FACE_OUTER_BOUND('',#1753,.T.);
#1218=FACE_OUTER_BOUND('',#1754,.T.);
#1219=FACE_OUTER_BOUND('',#1755,.T.);
#1220=FACE_OUTER_BOUND('',#1756,.T.);
#1221=FACE_OUTER_BOUND('',#1757,.T.);
#1222=FACE_OUTER_BOUND('',#1758,.T.);
#1223=FACE_OUTER_BOUND('',#1759,.T.);
#1224=FACE_OUTER_BOUND('',#1760,.T.);
#1225=FACE_OUTER_BOUND('',#1761,.T.);
#1226=FACE_OUTER_BOUND('',#1762,.T.);
#1227=FACE_OUTER_BOUND('',#1763,.T.);
#1228=FACE_OUTER_BOUND('',#1764,.T.);
#1229=FACE_OUTER_BOUND('',#1765,.T.);
#1230=FACE_OUTER_BOUND('',#1766,.T.);
#1231=FACE_OUTER_BOUND('',#1767,.T.);
#1232=FACE_OUTER_BOUND('',#1768,.T.);
#1233=FACE_OUTER_BOUND('',#1770,.T.);
#1234=FACE_OUTER_BOUND('',#1771,.T.);
#1235=FACE_OUTER_BOUND('',#1773,.T.);
#1236=FACE_OUTER_BOUND('',#1774,.T.);
#1237=FACE_OUTER_BOUND('',#1775,.T.);
#1238=FACE_OUTER_BOUND('',#1776,.T.);
#1239=FACE_OUTER_BOUND('',#1777,.T.);
#1240=FACE_OUTER_BOUND('',#1779,.T.);
#1241=FACE_OUTER_BOUND('',#1780,.T.);
#1242=FACE_OUTER_BOUND('',#1781,.T.);
#1243=FACE_OUTER_BOUND('',#1782,.T.);
#1244=FACE_OUTER_BOUND('',#1783,.T.);
#1245=FACE_OUTER_BOUND('',#1784,.T.);
#1246=FACE_OUTER_BOUND('',#1785,.T.);
#1247=FACE_OUTER_BOUND('',#1786,.T.);
#1248=FACE_OUTER_BOUND('',#1787,.T.);
#1249=FACE_OUTER_BOUND('',#1788,.T.);
#1250=FACE_OUTER_BOUND('',#1789,.T.);
#1251=FACE_OUTER_BOUND('',#1790,.T.);
#1252=FACE_OUTER_BOUND('',#1791,.T.);
#1253=FACE_OUTER_BOUND('',#1792,.T.);
#1254=FACE_OUTER_BOUND('',#1793,.T.);
#1255=FACE_OUTER_BOUND('',#1795,.T.);
#1256=FACE_OUTER_BOUND('',#1796,.T.);
#1257=FACE_OUTER_BOUND('',#1798,.T.);
#1258=FACE_OUTER_BOUND('',#1799,.T.);
#1259=FACE_OUTER_BOUND('',#1800,.T.);
#1260=FACE_OUTER_BOUND('',#1801,.T.);
#1261=FACE_OUTER_BOUND('',#1802,.T.);
#1262=FACE_OUTER_BOUND('',#1804,.T.);
#1263=FACE_OUTER_BOUND('',#1805,.T.);
#1264=FACE_OUTER_BOUND('',#1806,.T.);
#1265=FACE_OUTER_BOUND('',#1807,.T.);
#1266=FACE_OUTER_BOUND('',#1808,.T.);
#1267=FACE_OUTER_BOUND('',#1809,.T.);
#1268=FACE_OUTER_BOUND('',#1810,.T.);
#1269=FACE_OUTER_BOUND('',#1811,.T.);
#1270=FACE_OUTER_BOUND('',#1812,.T.);
#1271=FACE_OUTER_BOUND('',#1813,.T.);
#1272=FACE_OUTER_BOUND('',#1814,.T.);
#1273=FACE_OUTER_BOUND('',#1815,.T.);
#1274=FACE_OUTER_BOUND('',#1816,.T.);
#1275=FACE_OUTER_BOUND('',#1817,.T.);
#1276=FACE_OUTER_BOUND('',#1818,.T.);
#1277=FACE_OUTER_BOUND('',#1820,.T.);
#1278=FACE_OUTER_BOUND('',#1822,.T.);
#1279=FACE_OUTER_BOUND('',#1823,.T.);
#1280=FACE_OUTER_BOUND('',#1824,.T.);
#1281=FACE_OUTER_BOUND('',#1825,.T.);
#1282=FACE_OUTER_BOUND('',#1826,.T.);
#1283=FACE_OUTER_BOUND('',#1828,.T.);
#1284=FACE_OUTER_BOUND('',#1829,.T.);
#1285=FACE_OUTER_BOUND('',#1830,.T.);
#1286=FACE_OUTER_BOUND('',#1831,.T.);
#1287=FACE_OUTER_BOUND('',#1832,.T.);
#1288=FACE_OUTER_BOUND('',#1833,.T.);
#1289=FACE_OUTER_BOUND('',#1834,.T.);
#1290=FACE_OUTER_BOUND('',#1835,.T.);
#1291=FACE_OUTER_BOUND('',#1836,.T.);
#1292=FACE_OUTER_BOUND('',#1837,.T.);
#1293=FACE_OUTER_BOUND('',#1838,.T.);
#1294=FACE_OUTER_BOUND('',#1839,.T.);
#1295=EDGE_LOOP('',(#5813,#5814,#5815,#5816));
#1296=EDGE_LOOP('',(#5817,#5818,#5819,#5820));
#1297=EDGE_LOOP('',(#5821,#5822,#5823,#5824));
#1298=EDGE_LOOP('',(#5825,#5826,#5827,#5828));
#1299=EDGE_LOOP('',(#5829,#5830,#5831,#5832));
#1300=EDGE_LOOP('',(#5833,#5834,#5835,#5836));
#1301=EDGE_LOOP('',(#5837,#5838,#5839,#5840));
#1302=EDGE_LOOP('',(#5841,#5842,#5843,#5844));
#1303=EDGE_LOOP('',(#5845,#5846,#5847,#5848));
#1304=EDGE_LOOP('',(#5849,#5850,#5851,#5852));
#1305=EDGE_LOOP('',(#5853,#5854,#5855,#5856));
#1306=EDGE_LOOP('',(#5857,#5858,#5859,#5860));
#1307=EDGE_LOOP('',(#5861,#5862,#5863,#5864));
#1308=EDGE_LOOP('',(#5865,#5866,#5867,#5868));
#1309=EDGE_LOOP('',(#5869,#5870,#5871,#5872));
#1310=EDGE_LOOP('',(#5873,#5874,#5875,#5876));
#1311=EDGE_LOOP('',(#5877,#5878,#5879,#5880));
#1312=EDGE_LOOP('',(#5881,#5882,#5883,#5884));
#1313=EDGE_LOOP('',(#5885,#5886,#5887,#5888));
#1314=EDGE_LOOP('',(#5889));
#1315=EDGE_LOOP('',(#5890));
#1316=EDGE_LOOP('',(#5891));
#1317=EDGE_LOOP('',(#5892));
#1318=EDGE_LOOP('',(#5893));
#1319=EDGE_LOOP('',(#5894));
#1320=EDGE_LOOP('',(#5895));
#1321=EDGE_LOOP('',(#5896));
#1322=EDGE_LOOP('',(#5897));
#1323=EDGE_LOOP('',(#5898));
#1324=EDGE_LOOP('',(#5899));
#1325=EDGE_LOOP('',(#5900));
#1326=EDGE_LOOP('',(#5901));
#1327=EDGE_LOOP('',(#5902));
#1328=EDGE_LOOP('',(#5903,#5904,#5905,#5906));
#1329=EDGE_LOOP('',(#5907));
#1330=EDGE_LOOP('',(#5908));
#1331=EDGE_LOOP('',(#5909));
#1332=EDGE_LOOP('',(#5910));
#1333=EDGE_LOOP('',(#5911));
#1334=EDGE_LOOP('',(#5912));
#1335=EDGE_LOOP('',(#5913));
#1336=EDGE_LOOP('',(#5914));
#1337=EDGE_LOOP('',(#5915));
#1338=EDGE_LOOP('',(#5916));
#1339=EDGE_LOOP('',(#5917));
#1340=EDGE_LOOP('',(#5918));
#1341=EDGE_LOOP('',(#5919));
#1342=EDGE_LOOP('',(#5920));
#1343=EDGE_LOOP('',(#5921,#5922,#5923,#5924));
#1344=EDGE_LOOP('',(#5925));
#1345=EDGE_LOOP('',(#5926));
#1346=EDGE_LOOP('',(#5927,#5928,#5929,#5930));
#1347=EDGE_LOOP('',(#5931));
#1348=EDGE_LOOP('',(#5932));
#1349=EDGE_LOOP('',(#5933,#5934,#5935,#5936));
#1350=EDGE_LOOP('',(#5937,#5938,#5939,#5940));
#1351=EDGE_LOOP('',(#5941,#5942,#5943,#5944));
#1352=EDGE_LOOP('',(#5945,#5946,#5947,#5948));
#1353=EDGE_LOOP('',(#5949,#5950,#5951,#5952));
#1354=EDGE_LOOP('',(#5953,#5954,#5955,#5956));
#1355=EDGE_LOOP('',(#5957,#5958,#5959,#5960));
#1356=EDGE_LOOP('',(#5961));
#1357=EDGE_LOOP('',(#5962));
#1358=EDGE_LOOP('',(#5963,#5964,#5965,#5966));
#1359=EDGE_LOOP('',(#5967));
#1360=EDGE_LOOP('',(#5968));
#1361=EDGE_LOOP('',(#5969,#5970,#5971,#5972));
#1362=EDGE_LOOP('',(#5973,#5974,#5975,#5976));
#1363=EDGE_LOOP('',(#5977,#5978,#5979,#5980));
#1364=EDGE_LOOP('',(#5981,#5982,#5983,#5984));
#1365=EDGE_LOOP('',(#5985,#5986,#5987,#5988));
#1366=EDGE_LOOP('',(#5989,#5990,#5991,#5992));
#1367=EDGE_LOOP('',(#5993,#5994,#5995,#5996));
#1368=EDGE_LOOP('',(#5997));
#1369=EDGE_LOOP('',(#5998));
#1370=EDGE_LOOP('',(#5999,#6000,#6001,#6002));
#1371=EDGE_LOOP('',(#6003));
#1372=EDGE_LOOP('',(#6004));
#1373=EDGE_LOOP('',(#6005,#6006,#6007,#6008));
#1374=EDGE_LOOP('',(#6009,#6010,#6011,#6012));
#1375=EDGE_LOOP('',(#6013,#6014,#6015,#6016));
#1376=EDGE_LOOP('',(#6017,#6018,#6019,#6020));
#1377=EDGE_LOOP('',(#6021,#6022,#6023,#6024));
#1378=EDGE_LOOP('',(#6025,#6026,#6027,#6028));
#1379=EDGE_LOOP('',(#6029,#6030,#6031,#6032));
#1380=EDGE_LOOP('',(#6033));
#1381=EDGE_LOOP('',(#6034));
#1382=EDGE_LOOP('',(#6035,#6036,#6037,#6038));
#1383=EDGE_LOOP('',(#6039));
#1384=EDGE_LOOP('',(#6040));
#1385=EDGE_LOOP('',(#6041,#6042,#6043,#6044));
#1386=EDGE_LOOP('',(#6045,#6046,#6047,#6048));
#1387=EDGE_LOOP('',(#6049,#6050,#6051,#6052));
#1388=EDGE_LOOP('',(#6053,#6054,#6055,#6056));
#1389=EDGE_LOOP('',(#6057,#6058,#6059,#6060));
#1390=EDGE_LOOP('',(#6061,#6062,#6063,#6064));
#1391=EDGE_LOOP('',(#6065,#6066,#6067,#6068));
#1392=EDGE_LOOP('',(#6069,#6070,#6071,#6072));
#1393=EDGE_LOOP('',(#6073,#6074,#6075,#6076));
#1394=EDGE_LOOP('',(#6077,#6078,#6079,#6080));
#1395=EDGE_LOOP('',(#6081,#6082,#6083,#6084));
#1396=EDGE_LOOP('',(#6085,#6086,#6087,#6088));
#1397=EDGE_LOOP('',(#6089,#6090,#6091,#6092));
#1398=EDGE_LOOP('',(#6093,#6094,#6095,#6096));
#1399=EDGE_LOOP('',(#6097,#6098,#6099,#6100));
#1400=EDGE_LOOP('',(#6101,#6102,#6103,#6104));
#1401=EDGE_LOOP('',(#6105,#6106,#6107,#6108));
#1402=EDGE_LOOP('',(#6109,#6110,#6111,#6112));
#1403=EDGE_LOOP('',(#6113,#6114,#6115,#6116));
#1404=EDGE_LOOP('',(#6117,#6118,#6119,#6120));
#1405=EDGE_LOOP('',(#6121,#6122,#6123,#6124));
#1406=EDGE_LOOP('',(#6125,#6126,#6127,#6128));
#1407=EDGE_LOOP('',(#6129,#6130,#6131,#6132));
#1408=EDGE_LOOP('',(#6133,#6134,#6135,#6136));
#1409=EDGE_LOOP('',(#6137,#6138,#6139,#6140));
#1410=EDGE_LOOP('',(#6141,#6142,#6143,#6144));
#1411=EDGE_LOOP('',(#6145,#6146,#6147,#6148));
#1412=EDGE_LOOP('',(#6149,#6150,#6151,#6152));
#1413=EDGE_LOOP('',(#6153,#6154,#6155,#6156));
#1414=EDGE_LOOP('',(#6157,#6158,#6159,#6160));
#1415=EDGE_LOOP('',(#6161,#6162,#6163,#6164));
#1416=EDGE_LOOP('',(#6165,#6166,#6167,#6168));
#1417=EDGE_LOOP('',(#6169,#6170,#6171,#6172));
#1418=EDGE_LOOP('',(#6173,#6174,#6175,#6176));
#1419=EDGE_LOOP('',(#6177,#6178,#6179,#6180));
#1420=EDGE_LOOP('',(#6181,#6182,#6183,#6184));
#1421=EDGE_LOOP('',(#6185,#6186,#6187,#6188));
#1422=EDGE_LOOP('',(#6189,#6190,#6191,#6192));
#1423=EDGE_LOOP('',(#6193,#6194,#6195,#6196));
#1424=EDGE_LOOP('',(#6197,#6198,#6199,#6200));
#1425=EDGE_LOOP('',(#6201,#6202,#6203,#6204));
#1426=EDGE_LOOP('',(#6205,#6206,#6207,#6208));
#1427=EDGE_LOOP('',(#6209,#6210,#6211,#6212));
#1428=EDGE_LOOP('',(#6213,#6214,#6215,#6216));
#1429=EDGE_LOOP('',(#6217,#6218,#6219,#6220));
#1430=EDGE_LOOP('',(#6221,#6222,#6223,#6224));
#1431=EDGE_LOOP('',(#6225,#6226,#6227,#6228));
#1432=EDGE_LOOP('',(#6229,#6230,#6231,#6232));
#1433=EDGE_LOOP('',(#6233,#6234,#6235,#6236));
#1434=EDGE_LOOP('',(#6237,#6238,#6239,#6240));
#1435=EDGE_LOOP('',(#6241,#6242,#6243,#6244));
#1436=EDGE_LOOP('',(#6245,#6246,#6247,#6248));
#1437=EDGE_LOOP('',(#6249,#6250,#6251,#6252));
#1438=EDGE_LOOP('',(#6253,#6254,#6255,#6256));
#1439=EDGE_LOOP('',(#6257,#6258,#6259,#6260));
#1440=EDGE_LOOP('',(#6261,#6262,#6263,#6264));
#1441=EDGE_LOOP('',(#6265,#6266,#6267,#6268));
#1442=EDGE_LOOP('',(#6269,#6270,#6271,#6272));
#1443=EDGE_LOOP('',(#6273,#6274,#6275,#6276));
#1444=EDGE_LOOP('',(#6277,#6278,#6279,#6280));
#1445=EDGE_LOOP('',(#6281,#6282,#6283,#6284));
#1446=EDGE_LOOP('',(#6285,#6286,#6287,#6288));
#1447=EDGE_LOOP('',(#6289,#6290,#6291,#6292));
#1448=EDGE_LOOP('',(#6293,#6294,#6295,#6296));
#1449=EDGE_LOOP('',(#6297,#6298,#6299,#6300));
#1450=EDGE_LOOP('',(#6301,#6302,#6303,#6304));
#1451=EDGE_LOOP('',(#6305,#6306,#6307,#6308));
#1452=EDGE_LOOP('',(#6309,#6310,#6311,#6312));
#1453=EDGE_LOOP('',(#6313,#6314,#6315,#6316));
#1454=EDGE_LOOP('',(#6317,#6318,#6319,#6320));
#1455=EDGE_LOOP('',(#6321,#6322,#6323,#6324));
#1456=EDGE_LOOP('',(#6325,#6326,#6327,#6328));
#1457=EDGE_LOOP('',(#6329,#6330,#6331,#6332));
#1458=EDGE_LOOP('',(#6333,#6334,#6335,#6336));
#1459=EDGE_LOOP('',(#6337,#6338,#6339,#6340));
#1460=EDGE_LOOP('',(#6341,#6342,#6343,#6344));
#1461=EDGE_LOOP('',(#6345,#6346,#6347,#6348));
#1462=EDGE_LOOP('',(#6349,#6350,#6351,#6352));
#1463=EDGE_LOOP('',(#6353,#6354,#6355,#6356));
#1464=EDGE_LOOP('',(#6357,#6358,#6359,#6360));
#1465=EDGE_LOOP('',(#6361,#6362,#6363,#6364));
#1466=EDGE_LOOP('',(#6365,#6366,#6367,#6368));
#1467=EDGE_LOOP('',(#6369,#6370,#6371,#6372));
#1468=EDGE_LOOP('',(#6373,#6374,#6375,#6376));
#1469=EDGE_LOOP('',(#6377,#6378,#6379,#6380));
#1470=EDGE_LOOP('',(#6381,#6382,#6383,#6384));
#1471=EDGE_LOOP('',(#6385,#6386,#6387,#6388));
#1472=EDGE_LOOP('',(#6389,#6390,#6391,#6392));
#1473=EDGE_LOOP('',(#6393,#6394,#6395,#6396));
#1474=EDGE_LOOP('',(#6397,#6398,#6399,#6400));
#1475=EDGE_LOOP('',(#6401,#6402,#6403,#6404));
#1476=EDGE_LOOP('',(#6405,#6406,#6407,#6408));
#1477=EDGE_LOOP('',(#6409,#6410,#6411,#6412));
#1478=EDGE_LOOP('',(#6413,#6414,#6415,#6416));
#1479=EDGE_LOOP('',(#6417,#6418,#6419,#6420));
#1480=EDGE_LOOP('',(#6421,#6422,#6423,#6424));
#1481=EDGE_LOOP('',(#6425,#6426,#6427,#6428));
#1482=EDGE_LOOP('',(#6429,#6430,#6431,#6432));
#1483=EDGE_LOOP('',(#6433,#6434,#6435,#6436));
#1484=EDGE_LOOP('',(#6437,#6438,#6439,#6440));
#1485=EDGE_LOOP('',(#6441,#6442,#6443,#6444));
#1486=EDGE_LOOP('',(#6445,#6446,#6447,#6448));
#1487=EDGE_LOOP('',(#6449,#6450,#6451,#6452));
#1488=EDGE_LOOP('',(#6453,#6454,#6455,#6456));
#1489=EDGE_LOOP('',(#6457,#6458,#6459,#6460));
#1490=EDGE_LOOP('',(#6461,#6462,#6463,#6464));
#1491=EDGE_LOOP('',(#6465,#6466,#6467,#6468));
#1492=EDGE_LOOP('',(#6469,#6470,#6471,#6472));
#1493=EDGE_LOOP('',(#6473,#6474,#6475,#6476));
#1494=EDGE_LOOP('',(#6477,#6478,#6479,#6480));
#1495=EDGE_LOOP('',(#6481,#6482,#6483,#6484));
#1496=EDGE_LOOP('',(#6485,#6486,#6487,#6488));
#1497=EDGE_LOOP('',(#6489,#6490,#6491,#6492));
#1498=EDGE_LOOP('',(#6493,#6494,#6495,#6496));
#1499=EDGE_LOOP('',(#6497,#6498,#6499,#6500));
#1500=EDGE_LOOP('',(#6501,#6502,#6503,#6504));
#1501=EDGE_LOOP('',(#6505,#6506,#6507,#6508));
#1502=EDGE_LOOP('',(#6509,#6510,#6511,#6512));
#1503=EDGE_LOOP('',(#6513,#6514,#6515,#6516));
#1504=EDGE_LOOP('',(#6517,#6518,#6519,#6520));
#1505=EDGE_LOOP('',(#6521,#6522,#6523,#6524));
#1506=EDGE_LOOP('',(#6525,#6526,#6527,#6528));
#1507=EDGE_LOOP('',(#6529,#6530,#6531,#6532,#6533,#6534,#6535,#6536,#6537,
#6538,#6539,#6540,#6541,#6542,#6543,#6544,#6545,#6546,#6547,#6548,#6549,
#6550,#6551,#6552,#6553,#6554,#6555,#6556,#6557,#6558,#6559,#6560,#6561,
#6562,#6563,#6564,#6565,#6566,#6567,#6568,#6569,#6570,#6571,#6572,#6573,
#6574,#6575,#6576,#6577,#6578,#6579,#6580,#6581,#6582,#6583,#6584,#6585,
#6586,#6587,#6588,#6589,#6590,#6591,#6592,#6593,#6594,#6595,#6596,#6597,
#6598,#6599,#6600,#6601,#6602,#6603,#6604,#6605,#6606,#6607,#6608,#6609,
#6610,#6611,#6612,#6613,#6614,#6615,#6616,#6617,#6618,#6619,#6620,#6621,
#6622,#6623,#6624,#6625,#6626,#6627,#6628,#6629,#6630,#6631,#6632,#6633,
#6634,#6635,#6636,#6637,#6638,#6639,#6640,#6641,#6642,#6643,#6644,#6645,
#6646,#6647,#6648));
#1508=EDGE_LOOP('',(#6649));
#1509=EDGE_LOOP('',(#6650));
#1510=EDGE_LOOP('',(#6651,#6652,#6653,#6654));
#1511=EDGE_LOOP('',(#6655,#6656,#6657,#6658));
#1512=EDGE_LOOP('',(#6659,#6660,#6661,#6662));
#1513=EDGE_LOOP('',(#6663,#6664,#6665,#6666));
#1514=EDGE_LOOP('',(#6667,#6668,#6669,#6670,#6671,#6672,#6673,#6674,#6675,
#6676,#6677,#6678,#6679,#6680,#6681,#6682,#6683,#6684,#6685,#6686,#6687,
#6688,#6689,#6690,#6691,#6692,#6693,#6694,#6695,#6696,#6697,#6698,#6699,
#6700,#6701,#6702,#6703,#6704,#6705,#6706,#6707,#6708,#6709,#6710,#6711,
#6712,#6713,#6714,#6715,#6716,#6717,#6718,#6719,#6720,#6721,#6722,#6723,
#6724,#6725,#6726,#6727,#6728,#6729,#6730,#6731,#6732,#6733,#6734,#6735,
#6736,#6737,#6738,#6739,#6740,#6741,#6742,#6743,#6744,#6745,#6746,#6747,
#6748,#6749,#6750,#6751,#6752,#6753,#6754,#6755,#6756,#6757,#6758,#6759,
#6760,#6761,#6762,#6763,#6764,#6765,#6766,#6767,#6768,#6769,#6770,#6771,
#6772,#6773,#6774,#6775,#6776,#6777,#6778,#6779,#6780,#6781,#6782,#6783,
#6784,#6785,#6786));
#1515=EDGE_LOOP('',(#6787,#6788,#6789,#6790));
#1516=EDGE_LOOP('',(#6791,#6792,#6793,#6794));
#1517=EDGE_LOOP('',(#6795));
#1518=EDGE_LOOP('',(#6796));
#1519=EDGE_LOOP('',(#6797,#6798,#6799,#6800));
#1520=EDGE_LOOP('',(#6801,#6802,#6803,#6804));
#1521=EDGE_LOOP('',(#6805,#6806,#6807,#6808));
#1522=EDGE_LOOP('',(#6809,#6810,#6811,#6812));
#1523=EDGE_LOOP('',(#6813,#6814,#6815,#6816));
#1524=EDGE_LOOP('',(#6817,#6818,#6819,#6820));
#1525=EDGE_LOOP('',(#6821,#6822,#6823,#6824));
#1526=EDGE_LOOP('',(#6825,#6826,#6827,#6828));
#1527=EDGE_LOOP('',(#6829,#6830,#6831,#6832));
#1528=EDGE_LOOP('',(#6833,#6834,#6835,#6836));
#1529=EDGE_LOOP('',(#6837,#6838,#6839,#6840));
#1530=EDGE_LOOP('',(#6841,#6842,#6843,#6844));
#1531=EDGE_LOOP('',(#6845,#6846,#6847,#6848));
#1532=EDGE_LOOP('',(#6849,#6850,#6851,#6852));
#1533=EDGE_LOOP('',(#6853,#6854,#6855,#6856));
#1534=EDGE_LOOP('',(#6857,#6858,#6859,#6860));
#1535=EDGE_LOOP('',(#6861,#6862,#6863,#6864));
#1536=EDGE_LOOP('',(#6865,#6866,#6867,#6868));
#1537=EDGE_LOOP('',(#6869,#6870,#6871,#6872));
#1538=EDGE_LOOP('',(#6873,#6874,#6875,#6876));
#1539=EDGE_LOOP('',(#6877,#6878,#6879,#6880));
#1540=EDGE_LOOP('',(#6881,#6882,#6883,#6884));
#1541=EDGE_LOOP('',(#6885,#6886,#6887,#6888));
#1542=EDGE_LOOP('',(#6889,#6890,#6891,#6892));
#1543=EDGE_LOOP('',(#6893,#6894,#6895,#6896));
#1544=EDGE_LOOP('',(#6897));
#1545=EDGE_LOOP('',(#6898));
#1546=EDGE_LOOP('',(#6899,#6900,#6901,#6902));
#1547=EDGE_LOOP('',(#6903));
#1548=EDGE_LOOP('',(#6904));
#1549=EDGE_LOOP('',(#6905,#6906,#6907,#6908));
#1550=EDGE_LOOP('',(#6909));
#1551=EDGE_LOOP('',(#6910));
#1552=EDGE_LOOP('',(#6911,#6912,#6913,#6914));
#1553=EDGE_LOOP('',(#6915));
#1554=EDGE_LOOP('',(#6916));
#1555=EDGE_LOOP('',(#6917,#6918,#6919,#6920));
#1556=EDGE_LOOP('',(#6921,#6922,#6923,#6924));
#1557=EDGE_LOOP('',(#6925,#6926,#6927,#6928));
#1558=EDGE_LOOP('',(#6929,#6930,#6931,#6932));
#1559=EDGE_LOOP('',(#6933,#6934,#6935,#6936));
#1560=EDGE_LOOP('',(#6937,#6938,#6939,#6940));
#1561=EDGE_LOOP('',(#6941,#6942,#6943,#6944));
#1562=EDGE_LOOP('',(#6945,#6946,#6947,#6948));
#1563=EDGE_LOOP('',(#6949,#6950,#6951,#6952));
#1564=EDGE_LOOP('',(#6953));
#1565=EDGE_LOOP('',(#6954));
#1566=EDGE_LOOP('',(#6955));
#1567=EDGE_LOOP('',(#6956));
#1568=EDGE_LOOP('',(#6957,#6958,#6959,#6960));
#1569=EDGE_LOOP('',(#6961,#6962,#6963,#6964));
#1570=EDGE_LOOP('',(#6965,#6966,#6967,#6968));
#1571=EDGE_LOOP('',(#6969,#6970,#6971,#6972));
#1572=EDGE_LOOP('',(#6973,#6974,#6975,#6976));
#1573=EDGE_LOOP('',(#6977,#6978,#6979,#6980));
#1574=EDGE_LOOP('',(#6981));
#1575=EDGE_LOOP('',(#6982));
#1576=EDGE_LOOP('',(#6983));
#1577=EDGE_LOOP('',(#6984));
#1578=EDGE_LOOP('',(#6985,#6986,#6987,#6988));
#1579=EDGE_LOOP('',(#6989,#6990,#6991,#6992,#6993,#6994,#6995,#6996,#6997,
#6998,#6999,#7000));
#1580=EDGE_LOOP('',(#7001,#7002,#7003,#7004,#7005,#7006,#7007,#7008,#7009,
#7010,#7011,#7012));
#1581=EDGE_LOOP('',(#7013,#7014,#7015,#7016));
#1582=EDGE_LOOP('',(#7017,#7018,#7019,#7020));
#1583=EDGE_LOOP('',(#7021,#7022,#7023,#7024));
#1584=EDGE_LOOP('',(#7025,#7026,#7027,#7028));
#1585=EDGE_LOOP('',(#7029,#7030,#7031,#7032));
#1586=EDGE_LOOP('',(#7033,#7034,#7035,#7036));
#1587=EDGE_LOOP('',(#7037,#7038,#7039,#7040));
#1588=EDGE_LOOP('',(#7041,#7042,#7043,#7044));
#1589=EDGE_LOOP('',(#7045,#7046,#7047,#7048));
#1590=EDGE_LOOP('',(#7049,#7050,#7051,#7052));
#1591=EDGE_LOOP('',(#7053,#7054,#7055,#7056));
#1592=EDGE_LOOP('',(#7057,#7058,#7059,#7060));
#1593=EDGE_LOOP('',(#7061,#7062,#7063,#7064));
#1594=EDGE_LOOP('',(#7065,#7066,#7067,#7068));
#1595=EDGE_LOOP('',(#7069,#7070,#7071,#7072));
#1596=EDGE_LOOP('',(#7073,#7074,#7075,#7076));
#1597=EDGE_LOOP('',(#7077,#7078,#7079,#7080));
#1598=EDGE_LOOP('',(#7081,#7082,#7083,#7084));
#1599=EDGE_LOOP('',(#7085,#7086,#7087,#7088));
#1600=EDGE_LOOP('',(#7089,#7090,#7091,#7092));
#1601=EDGE_LOOP('',(#7093,#7094,#7095,#7096));
#1602=EDGE_LOOP('',(#7097,#7098,#7099,#7100));
#1603=EDGE_LOOP('',(#7101,#7102,#7103,#7104));
#1604=EDGE_LOOP('',(#7105,#7106,#7107,#7108));
#1605=EDGE_LOOP('',(#7109,#7110,#7111,#7112));
#1606=EDGE_LOOP('',(#7113,#7114,#7115,#7116));
#1607=EDGE_LOOP('',(#7117,#7118,#7119,#7120));
#1608=EDGE_LOOP('',(#7121,#7122,#7123,#7124));
#1609=EDGE_LOOP('',(#7125,#7126,#7127,#7128));
#1610=EDGE_LOOP('',(#7129,#7130,#7131,#7132));
#1611=EDGE_LOOP('',(#7133,#7134,#7135,#7136));
#1612=EDGE_LOOP('',(#7137,#7138,#7139,#7140));
#1613=EDGE_LOOP('',(#7141,#7142,#7143,#7144));
#1614=EDGE_LOOP('',(#7145,#7146,#7147,#7148));
#1615=EDGE_LOOP('',(#7149,#7150,#7151,#7152));
#1616=EDGE_LOOP('',(#7153,#7154,#7155,#7156));
#1617=EDGE_LOOP('',(#7157,#7158,#7159,#7160));
#1618=EDGE_LOOP('',(#7161,#7162,#7163,#7164));
#1619=EDGE_LOOP('',(#7165,#7166,#7167,#7168));
#1620=EDGE_LOOP('',(#7169,#7170,#7171,#7172));
#1621=EDGE_LOOP('',(#7173,#7174,#7175,#7176));
#1622=EDGE_LOOP('',(#7177,#7178,#7179,#7180));
#1623=EDGE_LOOP('',(#7181,#7182,#7183,#7184));
#1624=EDGE_LOOP('',(#7185,#7186,#7187,#7188));
#1625=EDGE_LOOP('',(#7189,#7190,#7191,#7192));
#1626=EDGE_LOOP('',(#7193,#7194,#7195,#7196,#7197,#7198,#7199,#7200,#7201,
#7202,#7203,#7204,#7205,#7206,#7207,#7208,#7209,#7210,#7211,#7212,#7213,
#7214,#7215,#7216,#7217,#7218,#7219,#7220,#7221,#7222,#7223,#7224,#7225,
#7226,#7227,#7228,#7229,#7230,#7231,#7232,#7233,#7234,#7235,#7236));
#1627=EDGE_LOOP('',(#7237));
#1628=EDGE_LOOP('',(#7238,#7239,#7240,#7241,#7242,#7243,#7244,#7245,#7246,
#7247,#7248,#7249,#7250,#7251,#7252,#7253,#7254,#7255,#7256,#7257,#7258,
#7259,#7260,#7261,#7262,#7263,#7264,#7265,#7266,#7267,#7268,#7269,#7270,
#7271,#7272,#7273,#7274,#7275,#7276,#7277,#7278,#7279,#7280,#7281));
#1629=EDGE_LOOP('',(#7282));
#1630=EDGE_LOOP('',(#7283,#7284,#7285,#7286));
#1631=EDGE_LOOP('',(#7287,#7288,#7289,#7290));
#1632=EDGE_LOOP('',(#7291,#7292,#7293,#7294));
#1633=EDGE_LOOP('',(#7295));
#1634=EDGE_LOOP('',(#7296,#7297,#7298,#7299,#7300,#7301,#7302,#7303,#7304,
#7305));
#1635=EDGE_LOOP('',(#7306,#7307,#7308,#7309));
#1636=EDGE_LOOP('',(#7310,#7311,#7312,#7313));
#1637=EDGE_LOOP('',(#7314,#7315,#7316,#7317,#7318,#7319,#7320,#7321,#7322,
#7323));
#1638=EDGE_LOOP('',(#7324,#7325,#7326,#7327));
#1639=EDGE_LOOP('',(#7328,#7329,#7330,#7331,#7332,#7333));
#1640=EDGE_LOOP('',(#7334,#7335,#7336,#7337,#7338,#7339,#7340,#7341));
#1641=EDGE_LOOP('',(#7342,#7343,#7344,#7345,#7346));
#1642=EDGE_LOOP('',(#7347,#7348,#7349,#7350));
#1643=EDGE_LOOP('',(#7351,#7352,#7353,#7354,#7355,#7356));
#1644=EDGE_LOOP('',(#7357,#7358,#7359,#7360));
#1645=EDGE_LOOP('',(#7361,#7362,#7363,#7364));
#1646=EDGE_LOOP('',(#7365,#7366,#7367,#7368));
#1647=EDGE_LOOP('',(#7369,#7370,#7371,#7372));
#1648=EDGE_LOOP('',(#7373,#7374,#7375,#7376));
#1649=EDGE_LOOP('',(#7377,#7378,#7379,#7380));
#1650=EDGE_LOOP('',(#7381,#7382,#7383,#7384));
#1651=EDGE_LOOP('',(#7385,#7386,#7387,#7388,#7389,#7390));
#1652=EDGE_LOOP('',(#7391,#7392,#7393,#7394,#7395,#7396));
#1653=EDGE_LOOP('',(#7397));
#1654=EDGE_LOOP('',(#7398));
#1655=EDGE_LOOP('',(#7399,#7400,#7401,#7402));
#1656=EDGE_LOOP('',(#7403,#7404,#7405,#7406));
#1657=EDGE_LOOP('',(#7407,#7408,#7409,#7410));
#1658=EDGE_LOOP('',(#7411));
#1659=EDGE_LOOP('',(#7412));
#1660=EDGE_LOOP('',(#7413,#7414,#7415,#7416));
#1661=EDGE_LOOP('',(#7417,#7418,#7419,#7420));
#1662=EDGE_LOOP('',(#7421,#7422,#7423,#7424));
#1663=EDGE_LOOP('',(#7425,#7426,#7427,#7428));
#1664=EDGE_LOOP('',(#7429,#7430,#7431,#7432));
#1665=EDGE_LOOP('',(#7433,#7434,#7435,#7436));
#1666=EDGE_LOOP('',(#7437,#7438,#7439,#7440));
#1667=EDGE_LOOP('',(#7441,#7442,#7443,#7444));
#1668=EDGE_LOOP('',(#7445,#7446,#7447,#7448,#7449,#7450));
#1669=EDGE_LOOP('',(#7451,#7452,#7453,#7454,#7455,#7456));
#1670=EDGE_LOOP('',(#7457));
#1671=EDGE_LOOP('',(#7458));
#1672=EDGE_LOOP('',(#7459,#7460,#7461,#7462));
#1673=EDGE_LOOP('',(#7463,#7464,#7465,#7466));
#1674=EDGE_LOOP('',(#7467,#7468,#7469,#7470));
#1675=EDGE_LOOP('',(#7471));
#1676=EDGE_LOOP('',(#7472));
#1677=EDGE_LOOP('',(#7473,#7474,#7475,#7476));
#1678=EDGE_LOOP('',(#7477,#7478,#7479,#7480));
#1679=EDGE_LOOP('',(#7481,#7482,#7483,#7484));
#1680=EDGE_LOOP('',(#7485,#7486,#7487,#7488));
#1681=EDGE_LOOP('',(#7489,#7490,#7491,#7492));
#1682=EDGE_LOOP('',(#7493,#7494,#7495,#7496));
#1683=EDGE_LOOP('',(#7497,#7498,#7499,#7500));
#1684=EDGE_LOOP('',(#7501,#7502,#7503,#7504));
#1685=EDGE_LOOP('',(#7505,#7506,#7507,#7508));
#1686=EDGE_LOOP('',(#7509,#7510,#7511,#7512));
#1687=EDGE_LOOP('',(#7513,#7514,#7515,#7516));
#1688=EDGE_LOOP('',(#7517,#7518,#7519,#7520));
#1689=EDGE_LOOP('',(#7521,#7522,#7523,#7524));
#1690=EDGE_LOOP('',(#7525));
#1691=EDGE_LOOP('',(#7526));
#1692=EDGE_LOOP('',(#7527));
#1693=EDGE_LOOP('',(#7528));
#1694=EDGE_LOOP('',(#7529));
#1695=EDGE_LOOP('',(#7530));
#1696=EDGE_LOOP('',(#7531,#7532,#7533,#7534));
#1697=EDGE_LOOP('',(#7535));
#1698=EDGE_LOOP('',(#7536));
#1699=EDGE_LOOP('',(#7537));
#1700=EDGE_LOOP('',(#7538));
#1701=EDGE_LOOP('',(#7539));
#1702=EDGE_LOOP('',(#7540));
#1703=EDGE_LOOP('',(#7541,#7542,#7543,#7544));
#1704=EDGE_LOOP('',(#7545,#7546,#7547,#7548));
#1705=EDGE_LOOP('',(#7549));
#1706=EDGE_LOOP('',(#7550,#7551,#7552,#7553));
#1707=EDGE_LOOP('',(#7554,#7555,#7556,#7557));
#1708=EDGE_LOOP('',(#7558,#7559,#7560,#7561));
#1709=EDGE_LOOP('',(#7562,#7563,#7564,#7565));
#1710=EDGE_LOOP('',(#7566));
#1711=EDGE_LOOP('',(#7567,#7568,#7569,#7570));
#1712=EDGE_LOOP('',(#7571,#7572,#7573,#7574,#7575,#7576));
#1713=EDGE_LOOP('',(#7577,#7578,#7579,#7580,#7581,#7582));
#1714=EDGE_LOOP('',(#7583,#7584,#7585,#7586));
#1715=EDGE_LOOP('',(#7587,#7588,#7589,#7590));
#1716=EDGE_LOOP('',(#7591));
#1717=EDGE_LOOP('',(#7592));
#1718=EDGE_LOOP('',(#7593));
#1719=EDGE_LOOP('',(#7594));
#1720=EDGE_LOOP('',(#7595,#7596));
#1721=EDGE_LOOP('',(#7597,#7598,#7599,#7600,#7601,#7602,#7603,#7604));
#1722=EDGE_LOOP('',(#7605,#7606));
#1723=EDGE_LOOP('',(#7607,#7608,#7609,#7610,#7611,#7612,#7613,#7614));
#1724=EDGE_LOOP('',(#7615,#7616));
#1725=EDGE_LOOP('',(#7617,#7618,#7619,#7620,#7621,#7622,#7623,#7624));
#1726=EDGE_LOOP('',(#7625,#7626));
#1727=EDGE_LOOP('',(#7627,#7628,#7629,#7630,#7631,#7632,#7633,#7634));
#1728=EDGE_LOOP('',(#7635,#7636,#7637,#7638,#7639,#7640,#7641,#7642,#7643,
#7644,#7645,#7646));
#1729=EDGE_LOOP('',(#7647,#7648,#7649,#7650,#7651,#7652,#7653,#7654,#7655,
#7656,#7657,#7658));
#1730=EDGE_LOOP('',(#7659,#7660,#7661,#7662,#7663,#7664,#7665,#7666,#7667,
#7668,#7669,#7670));
#1731=EDGE_LOOP('',(#7671,#7672,#7673,#7674,#7675,#7676,#7677,#7678,#7679,
#7680));
#1732=EDGE_LOOP('',(#7681,#7682,#7683,#7684));
#1733=EDGE_LOOP('',(#7685,#7686,#7687,#7688));
#1734=EDGE_LOOP('',(#7689));
#1735=EDGE_LOOP('',(#7690));
#1736=EDGE_LOOP('',(#7691));
#1737=EDGE_LOOP('',(#7692));
#1738=EDGE_LOOP('',(#7693,#7694,#7695,#7696));
#1739=EDGE_LOOP('',(#7697,#7698,#7699,#7700,#7701,#7702,#7703,#7704,#7705,
#7706));
#1740=EDGE_LOOP('',(#7707,#7708,#7709,#7710));
#1741=EDGE_LOOP('',(#7711,#7712,#7713,#7714));
#1742=EDGE_LOOP('',(#7715,#7716,#7717,#7718));
#1743=EDGE_LOOP('',(#7719,#7720,#7721,#7722));
#1744=EDGE_LOOP('',(#7723,#7724,#7725,#7726));
#1745=EDGE_LOOP('',(#7727,#7728,#7729,#7730,#7731,#7732,#7733,#7734,#7735,
#7736,#7737,#7738));
#1746=EDGE_LOOP('',(#7739,#7740,#7741,#7742));
#1747=EDGE_LOOP('',(#7743,#7744,#7745,#7746));
#1748=EDGE_LOOP('',(#7747,#7748,#7749,#7750));
#1749=EDGE_LOOP('',(#7751,#7752,#7753,#7754));
#1750=EDGE_LOOP('',(#7755,#7756,#7757,#7758));
#1751=EDGE_LOOP('',(#7759,#7760,#7761,#7762));
#1752=EDGE_LOOP('',(#7763,#7764,#7765,#7766));
#1753=EDGE_LOOP('',(#7767,#7768,#7769,#7770));
#1754=EDGE_LOOP('',(#7771,#7772,#7773,#7774,#7775,#7776,#7777,#7778));
#1755=EDGE_LOOP('',(#7779,#7780,#7781,#7782,#7783,#7784,#7785,#7786));
#1756=EDGE_LOOP('',(#7787,#7788,#7789,#7790));
#1757=EDGE_LOOP('',(#7791,#7792,#7793,#7794));
#1758=EDGE_LOOP('',(#7795,#7796,#7797,#7798));
#1759=EDGE_LOOP('',(#7799,#7800,#7801,#7802));
#1760=EDGE_LOOP('',(#7803,#7804,#7805,#7806));
#1761=EDGE_LOOP('',(#7807,#7808,#7809,#7810));
#1762=EDGE_LOOP('',(#7811,#7812,#7813,#7814));
#1763=EDGE_LOOP('',(#7815,#7816,#7817,#7818));
#1764=EDGE_LOOP('',(#7819,#7820,#7821,#7822,#7823,#7824,#7825,#7826));
#1765=EDGE_LOOP('',(#7827,#7828,#7829,#7830,#7831,#7832,#7833,#7834));
#1766=EDGE_LOOP('',(#7835,#7836,#7837,#7838));
#1767=EDGE_LOOP('',(#7839,#7840,#7841,#7842));
#1768=EDGE_LOOP('',(#7843));
#1769=EDGE_LOOP('',(#7844));
#1770=EDGE_LOOP('',(#7845,#7846,#7847,#7848));
#1771=EDGE_LOOP('',(#7849));
#1772=EDGE_LOOP('',(#7850));
#1773=EDGE_LOOP('',(#7851));
#1774=EDGE_LOOP('',(#7852,#7853,#7854,#7855));
#1775=EDGE_LOOP('',(#7856,#7857,#7858,#7859));
#1776=EDGE_LOOP('',(#7860,#7861,#7862,#7863));
#1777=EDGE_LOOP('',(#7864));
#1778=EDGE_LOOP('',(#7865));
#1779=EDGE_LOOP('',(#7866,#7867,#7868,#7869));
#1780=EDGE_LOOP('',(#7870,#7871,#7872,#7873));
#1781=EDGE_LOOP('',(#7874,#7875,#7876,#7877));
#1782=EDGE_LOOP('',(#7878));
#1783=EDGE_LOOP('',(#7879,#7880,#7881,#7882));
#1784=EDGE_LOOP('',(#7883,#7884,#7885,#7886));
#1785=EDGE_LOOP('',(#7887,#7888,#7889,#7890));
#1786=EDGE_LOOP('',(#7891,#7892,#7893,#7894));
#1787=EDGE_LOOP('',(#7895,#7896,#7897,#7898));
#1788=EDGE_LOOP('',(#7899,#7900,#7901,#7902));
#1789=EDGE_LOOP('',(#7903,#7904,#7905,#7906,#7907,#7908));
#1790=EDGE_LOOP('',(#7909,#7910,#7911,#7912,#7913,#7914));
#1791=EDGE_LOOP('',(#7915,#7916,#7917,#7918));
#1792=EDGE_LOOP('',(#7919,#7920,#7921,#7922));
#1793=EDGE_LOOP('',(#7923));
#1794=EDGE_LOOP('',(#7924));
#1795=EDGE_LOOP('',(#7925,#7926,#7927,#7928));
#1796=EDGE_LOOP('',(#7929));
#1797=EDGE_LOOP('',(#7930));
#1798=EDGE_LOOP('',(#7931));
#1799=EDGE_LOOP('',(#7932,#7933,#7934,#7935));
#1800=EDGE_LOOP('',(#7936,#7937,#7938,#7939));
#1801=EDGE_LOOP('',(#7940,#7941,#7942,#7943));
#1802=EDGE_LOOP('',(#7944));
#1803=EDGE_LOOP('',(#7945));
#1804=EDGE_LOOP('',(#7946,#7947,#7948,#7949));
#1805=EDGE_LOOP('',(#7950,#7951,#7952,#7953));
#1806=EDGE_LOOP('',(#7954,#7955,#7956,#7957));
#1807=EDGE_LOOP('',(#7958));
#1808=EDGE_LOOP('',(#7959,#7960,#7961,#7962));
#1809=EDGE_LOOP('',(#7963,#7964,#7965,#7966));
#1810=EDGE_LOOP('',(#7967,#7968,#7969,#7970));
#1811=EDGE_LOOP('',(#7971,#7972,#7973,#7974));
#1812=EDGE_LOOP('',(#7975,#7976,#7977,#7978));
#1813=EDGE_LOOP('',(#7979,#7980,#7981,#7982));
#1814=EDGE_LOOP('',(#7983,#7984,#7985,#7986,#7987,#7988));
#1815=EDGE_LOOP('',(#7989,#7990,#7991,#7992,#7993,#7994));
#1816=EDGE_LOOP('',(#7995,#7996,#7997,#7998));
#1817=EDGE_LOOP('',(#7999,#8000,#8001,#8002));
#1818=EDGE_LOOP('',(#8003));
#1819=EDGE_LOOP('',(#8004));
#1820=EDGE_LOOP('',(#8005));
#1821=EDGE_LOOP('',(#8006));
#1822=EDGE_LOOP('',(#8007));
#1823=EDGE_LOOP('',(#8008,#8009,#8010,#8011));
#1824=EDGE_LOOP('',(#8012,#8013,#8014,#8015));
#1825=EDGE_LOOP('',(#8016,#8017,#8018,#8019));
#1826=EDGE_LOOP('',(#8020));
#1827=EDGE_LOOP('',(#8021));
#1828=EDGE_LOOP('',(#8022,#8023,#8024,#8025));
#1829=EDGE_LOOP('',(#8026,#8027,#8028,#8029));
#1830=EDGE_LOOP('',(#8030,#8031,#8032,#8033));
#1831=EDGE_LOOP('',(#8034));
#1832=EDGE_LOOP('',(#8035,#8036,#8037,#8038));
#1833=EDGE_LOOP('',(#8039,#8040,#8041,#8042));
#1834=EDGE_LOOP('',(#8043,#8044,#8045,#8046));
#1835=EDGE_LOOP('',(#8047,#8048,#8049,#8050));
#1836=EDGE_LOOP('',(#8051,#8052,#8053,#8054));
#1837=EDGE_LOOP('',(#8055,#8056,#8057,#8058));
#1838=EDGE_LOOP('',(#8059,#8060,#8061,#8062,#8063,#8064));
#1839=EDGE_LOOP('',(#8065,#8066,#8067,#8068,#8069,#8070));
#1840=LINE('',#12003,#2811);
#1841=LINE('',#12009,#2812);
#1842=LINE('',#12015,#2813);
#1843=LINE('',#12021,#2814);
#1844=LINE('',#12027,#2815);
#1845=LINE('',#12033,#2816);
#1846=LINE('',#12039,#2817);
#1847=LINE('',#12045,#2818);
#1848=LINE('',#12051,#2819);
#1849=LINE('',#12057,#2820);
#1850=LINE('',#12063,#2821);
#1851=LINE('',#12069,#2822);
#1852=LINE('',#12075,#2823);
#1853=LINE('',#12081,#2824);
#1854=LINE('',#12086,#2825);
#1855=LINE('',#12088,#2826);
#1856=LINE('',#12090,#2827);
#1857=LINE('',#12091,#2828);
#1858=LINE('',#12094,#2829);
#1859=LINE('',#12096,#2830);
#1860=LINE('',#12097,#2831);
#1861=LINE('',#12100,#2832);
#1862=LINE('',#12102,#2833);
#1863=LINE('',#12103,#2834);
#1864=LINE('',#12105,#2835);
#1865=LINE('',#12106,#2836);
#1866=LINE('',#12114,#2837);
#1867=LINE('',#12123,#2838);
#1868=LINE('',#12131,#2839);
#1869=LINE('',#12135,#2840);
#1870=LINE('',#12139,#2841);
#1871=LINE('',#12141,#2842);
#1872=LINE('',#12143,#2843);
#1873=LINE('',#12144,#2844);
#1874=LINE('',#12147,#2845);
#1875=LINE('',#12149,#2846);
#1876=LINE('',#12150,#2847);
#1877=LINE('',#12153,#2848);
#1878=LINE('',#12155,#2849);
#1879=LINE('',#12156,#2850);
#1880=LINE('',#12158,#2851);
#1881=LINE('',#12159,#2852);
#1882=LINE('',#12166,#2853);
#1883=LINE('',#12168,#2854);
#1884=LINE('',#12170,#2855);
#1885=LINE('',#12171,#2856);
#1886=LINE('',#12174,#2857);
#1887=LINE('',#12176,#2858);
#1888=LINE('',#12177,#2859);
#1889=LINE('',#12180,#2860);
#1890=LINE('',#12182,#2861);
#1891=LINE('',#12183,#2862);
#1892=LINE('',#12185,#2863);
#1893=LINE('',#12186,#2864);
#1894=LINE('',#12194,#2865);
#1895=LINE('',#12203,#2866);
#1896=LINE('',#12211,#2867);
#1897=LINE('',#12215,#2868);
#1898=LINE('',#12219,#2869);
#1899=LINE('',#12221,#2870);
#1900=LINE('',#12223,#2871);
#1901=LINE('',#12224,#2872);
#1902=LINE('',#12227,#2873);
#1903=LINE('',#12229,#2874);
#1904=LINE('',#12230,#2875);
#1905=LINE('',#12233,#2876);
#1906=LINE('',#12235,#2877);
#1907=LINE('',#12236,#2878);
#1908=LINE('',#12238,#2879);
#1909=LINE('',#12239,#2880);
#1910=LINE('',#12246,#2881);
#1911=LINE('',#12248,#2882);
#1912=LINE('',#12250,#2883);
#1913=LINE('',#12251,#2884);
#1914=LINE('',#12254,#2885);
#1915=LINE('',#12256,#2886);
#1916=LINE('',#12257,#2887);
#1917=LINE('',#12260,#2888);
#1918=LINE('',#12262,#2889);
#1919=LINE('',#12263,#2890);
#1920=LINE('',#12265,#2891);
#1921=LINE('',#12266,#2892);
#1922=LINE('',#12273,#2893);
#1923=LINE('',#12275,#2894);
#1924=LINE('',#12277,#2895);
#1925=LINE('',#12278,#2896);
#1926=LINE('',#12281,#2897);
#1927=LINE('',#12283,#2898);
#1928=LINE('',#12284,#2899);
#1929=LINE('',#12287,#2900);
#1930=LINE('',#12289,#2901);
#1931=LINE('',#12290,#2902);
#1932=LINE('',#12292,#2903);
#1933=LINE('',#12296,#2904);
#1934=LINE('',#12298,#2905);
#1935=LINE('',#12300,#2906);
#1936=LINE('',#12301,#2907);
#1937=LINE('',#12304,#2908);
#1938=LINE('',#12306,#2909);
#1939=LINE('',#12307,#2910);
#1940=LINE('',#12310,#2911);
#1941=LINE('',#12312,#2912);
#1942=LINE('',#12313,#2913);
#1943=LINE('',#12315,#2914);
#1944=LINE('',#12319,#2915);
#1945=LINE('',#12321,#2916);
#1946=LINE('',#12323,#2917);
#1947=LINE('',#12324,#2918);
#1948=LINE('',#12327,#2919);
#1949=LINE('',#12329,#2920);
#1950=LINE('',#12330,#2921);
#1951=LINE('',#12333,#2922);
#1952=LINE('',#12335,#2923);
#1953=LINE('',#12336,#2924);
#1954=LINE('',#12338,#2925);
#1955=LINE('',#12342,#2926);
#1956=LINE('',#12344,#2927);
#1957=LINE('',#12346,#2928);
#1958=LINE('',#12347,#2929);
#1959=LINE('',#12350,#2930);
#1960=LINE('',#12352,#2931);
#1961=LINE('',#12353,#2932);
#1962=LINE('',#12356,#2933);
#1963=LINE('',#12358,#2934);
#1964=LINE('',#12359,#2935);
#1965=LINE('',#12361,#2936);
#1966=LINE('',#12365,#2937);
#1967=LINE('',#12367,#2938);
#1968=LINE('',#12369,#2939);
#1969=LINE('',#12370,#2940);
#1970=LINE('',#12373,#2941);
#1971=LINE('',#12375,#2942);
#1972=LINE('',#12376,#2943);
#1973=LINE('',#12379,#2944);
#1974=LINE('',#12381,#2945);
#1975=LINE('',#12382,#2946);
#1976=LINE('',#12384,#2947);
#1977=LINE('',#12388,#2948);
#1978=LINE('',#12390,#2949);
#1979=LINE('',#12392,#2950);
#1980=LINE('',#12393,#2951);
#1981=LINE('',#12396,#2952);
#1982=LINE('',#12398,#2953);
#1983=LINE('',#12399,#2954);
#1984=LINE('',#12402,#2955);
#1985=LINE('',#12404,#2956);
#1986=LINE('',#12405,#2957);
#1987=LINE('',#12407,#2958);
#1988=LINE('',#12411,#2959);
#1989=LINE('',#12413,#2960);
#1990=LINE('',#12415,#2961);
#1991=LINE('',#12416,#2962);
#1992=LINE('',#12419,#2963);
#1993=LINE('',#12421,#2964);
#1994=LINE('',#12422,#2965);
#1995=LINE('',#12425,#2966);
#1996=LINE('',#12427,#2967);
#1997=LINE('',#12428,#2968);
#1998=LINE('',#12430,#2969);
#1999=LINE('',#12434,#2970);
#2000=LINE('',#12436,#2971);
#2001=LINE('',#12438,#2972);
#2002=LINE('',#12439,#2973);
#2003=LINE('',#12442,#2974);
#2004=LINE('',#12444,#2975);
#2005=LINE('',#12445,#2976);
#2006=LINE('',#12448,#2977);
#2007=LINE('',#12450,#2978);
#2008=LINE('',#12451,#2979);
#2009=LINE('',#12453,#2980);
#2010=LINE('',#12457,#2981);
#2011=LINE('',#12459,#2982);
#2012=LINE('',#12461,#2983);
#2013=LINE('',#12462,#2984);
#2014=LINE('',#12465,#2985);
#2015=LINE('',#12467,#2986);
#2016=LINE('',#12468,#2987);
#2017=LINE('',#12471,#2988);
#2018=LINE('',#12473,#2989);
#2019=LINE('',#12474,#2990);
#2020=LINE('',#12476,#2991);
#2021=LINE('',#12480,#2992);
#2022=LINE('',#12482,#2993);
#2023=LINE('',#12484,#2994);
#2024=LINE('',#12485,#2995);
#2025=LINE('',#12488,#2996);
#2026=LINE('',#12490,#2997);
#2027=LINE('',#12491,#2998);
#2028=LINE('',#12494,#2999);
#2029=LINE('',#12496,#3000);
#2030=LINE('',#12497,#3001);
#2031=LINE('',#12499,#3002);
#2032=LINE('',#12503,#3003);
#2033=LINE('',#12505,#3004);
#2034=LINE('',#12507,#3005);
#2035=LINE('',#12508,#3006);
#2036=LINE('',#12511,#3007);
#2037=LINE('',#12513,#3008);
#2038=LINE('',#12514,#3009);
#2039=LINE('',#12517,#3010);
#2040=LINE('',#12519,#3011);
#2041=LINE('',#12520,#3012);
#2042=LINE('',#12522,#3013);
#2043=LINE('',#12526,#3014);
#2044=LINE('',#12528,#3015);
#2045=LINE('',#12530,#3016);
#2046=LINE('',#12531,#3017);
#2047=LINE('',#12534,#3018);
#2048=LINE('',#12536,#3019);
#2049=LINE('',#12537,#3020);
#2050=LINE('',#12540,#3021);
#2051=LINE('',#12542,#3022);
#2052=LINE('',#12543,#3023);
#2053=LINE('',#12545,#3024);
#2054=LINE('',#12549,#3025);
#2055=LINE('',#12551,#3026);
#2056=LINE('',#12553,#3027);
#2057=LINE('',#12554,#3028);
#2058=LINE('',#12557,#3029);
#2059=LINE('',#12559,#3030);
#2060=LINE('',#12560,#3031);
#2061=LINE('',#12563,#3032);
#2062=LINE('',#12565,#3033);
#2063=LINE('',#12566,#3034);
#2064=LINE('',#12568,#3035);
#2065=LINE('',#12572,#3036);
#2066=LINE('',#12574,#3037);
#2067=LINE('',#12576,#3038);
#2068=LINE('',#12577,#3039);
#2069=LINE('',#12580,#3040);
#2070=LINE('',#12582,#3041);
#2071=LINE('',#12583,#3042);
#2072=LINE('',#12586,#3043);
#2073=LINE('',#12588,#3044);
#2074=LINE('',#12589,#3045);
#2075=LINE('',#12591,#3046);
#2076=LINE('',#12595,#3047);
#2077=LINE('',#12597,#3048);
#2078=LINE('',#12599,#3049);
#2079=LINE('',#12600,#3050);
#2080=LINE('',#12603,#3051);
#2081=LINE('',#12605,#3052);
#2082=LINE('',#12606,#3053);
#2083=LINE('',#12609,#3054);
#2084=LINE('',#12611,#3055);
#2085=LINE('',#12612,#3056);
#2086=LINE('',#12614,#3057);
#2087=LINE('',#12618,#3058);
#2088=LINE('',#12620,#3059);
#2089=LINE('',#12622,#3060);
#2090=LINE('',#12623,#3061);
#2091=LINE('',#12626,#3062);
#2092=LINE('',#12628,#3063);
#2093=LINE('',#12629,#3064);
#2094=LINE('',#12632,#3065);
#2095=LINE('',#12634,#3066);
#2096=LINE('',#12635,#3067);
#2097=LINE('',#12637,#3068);
#2098=LINE('',#12641,#3069);
#2099=LINE('',#12643,#3070);
#2100=LINE('',#12645,#3071);
#2101=LINE('',#12646,#3072);
#2102=LINE('',#12649,#3073);
#2103=LINE('',#12651,#3074);
#2104=LINE('',#12652,#3075);
#2105=LINE('',#12655,#3076);
#2106=LINE('',#12657,#3077);
#2107=LINE('',#12658,#3078);
#2108=LINE('',#12660,#3079);
#2109=LINE('',#12664,#3080);
#2110=LINE('',#12666,#3081);
#2111=LINE('',#12668,#3082);
#2112=LINE('',#12669,#3083);
#2113=LINE('',#12672,#3084);
#2114=LINE('',#12674,#3085);
#2115=LINE('',#12675,#3086);
#2116=LINE('',#12678,#3087);
#2117=LINE('',#12680,#3088);
#2118=LINE('',#12681,#3089);
#2119=LINE('',#12683,#3090);
#2120=LINE('',#12687,#3091);
#2121=LINE('',#12689,#3092);
#2122=LINE('',#12691,#3093);
#2123=LINE('',#12692,#3094);
#2124=LINE('',#12695,#3095);
#2125=LINE('',#12697,#3096);
#2126=LINE('',#12698,#3097);
#2127=LINE('',#12701,#3098);
#2128=LINE('',#12703,#3099);
#2129=LINE('',#12704,#3100);
#2130=LINE('',#12706,#3101);
#2131=LINE('',#12710,#3102);
#2132=LINE('',#12712,#3103);
#2133=LINE('',#12714,#3104);
#2134=LINE('',#12715,#3105);
#2135=LINE('',#12718,#3106);
#2136=LINE('',#12720,#3107);
#2137=LINE('',#12721,#3108);
#2138=LINE('',#12724,#3109);
#2139=LINE('',#12726,#3110);
#2140=LINE('',#12727,#3111);
#2141=LINE('',#12729,#3112);
#2142=LINE('',#12733,#3113);
#2143=LINE('',#12735,#3114);
#2144=LINE('',#12737,#3115);
#2145=LINE('',#12738,#3116);
#2146=LINE('',#12741,#3117);
#2147=LINE('',#12743,#3118);
#2148=LINE('',#12744,#3119);
#2149=LINE('',#12747,#3120);
#2150=LINE('',#12749,#3121);
#2151=LINE('',#12750,#3122);
#2152=LINE('',#12752,#3123);
#2153=LINE('',#12756,#3124);
#2154=LINE('',#12758,#3125);
#2155=LINE('',#12760,#3126);
#2156=LINE('',#12761,#3127);
#2157=LINE('',#12764,#3128);
#2158=LINE('',#12766,#3129);
#2159=LINE('',#12767,#3130);
#2160=LINE('',#12770,#3131);
#2161=LINE('',#12772,#3132);
#2162=LINE('',#12773,#3133);
#2163=LINE('',#12775,#3134);
#2164=LINE('',#12779,#3135);
#2165=LINE('',#12781,#3136);
#2166=LINE('',#12783,#3137);
#2167=LINE('',#12784,#3138);
#2168=LINE('',#12787,#3139);
#2169=LINE('',#12789,#3140);
#2170=LINE('',#12790,#3141);
#2171=LINE('',#12793,#3142);
#2172=LINE('',#12795,#3143);
#2173=LINE('',#12796,#3144);
#2174=LINE('',#12798,#3145);
#2175=LINE('',#12802,#3146);
#2176=LINE('',#12804,#3147);
#2177=LINE('',#12806,#3148);
#2178=LINE('',#12807,#3149);
#2179=LINE('',#12810,#3150);
#2180=LINE('',#12812,#3151);
#2181=LINE('',#12813,#3152);
#2182=LINE('',#12816,#3153);
#2183=LINE('',#12818,#3154);
#2184=LINE('',#12819,#3155);
#2185=LINE('',#12821,#3156);
#2186=LINE('',#12825,#3157);
#2187=LINE('',#12827,#3158);
#2188=LINE('',#12829,#3159);
#2189=LINE('',#12830,#3160);
#2190=LINE('',#12833,#3161);
#2191=LINE('',#12835,#3162);
#2192=LINE('',#12836,#3163);
#2193=LINE('',#12839,#3164);
#2194=LINE('',#12841,#3165);
#2195=LINE('',#12842,#3166);
#2196=LINE('',#12844,#3167);
#2197=LINE('',#12848,#3168);
#2198=LINE('',#12850,#3169);
#2199=LINE('',#12852,#3170);
#2200=LINE('',#12853,#3171);
#2201=LINE('',#12856,#3172);
#2202=LINE('',#12858,#3173);
#2203=LINE('',#12859,#3174);
#2204=LINE('',#12862,#3175);
#2205=LINE('',#12864,#3176);
#2206=LINE('',#12865,#3177);
#2207=LINE('',#12867,#3178);
#2208=LINE('',#12871,#3179);
#2209=LINE('',#12873,#3180);
#2210=LINE('',#12875,#3181);
#2211=LINE('',#12876,#3182);
#2212=LINE('',#12879,#3183);
#2213=LINE('',#12881,#3184);
#2214=LINE('',#12882,#3185);
#2215=LINE('',#12885,#3186);
#2216=LINE('',#12887,#3187);
#2217=LINE('',#12888,#3188);
#2218=LINE('',#12890,#3189);
#2219=LINE('',#12894,#3190);
#2220=LINE('',#12896,#3191);
#2221=LINE('',#12898,#3192);
#2222=LINE('',#12899,#3193);
#2223=LINE('',#12902,#3194);
#2224=LINE('',#12904,#3195);
#2225=LINE('',#12905,#3196);
#2226=LINE('',#12908,#3197);
#2227=LINE('',#12910,#3198);
#2228=LINE('',#12911,#3199);
#2229=LINE('',#12913,#3200);
#2230=LINE('',#12917,#3201);
#2231=LINE('',#12919,#3202);
#2232=LINE('',#12921,#3203);
#2233=LINE('',#12922,#3204);
#2234=LINE('',#12925,#3205);
#2235=LINE('',#12927,#3206);
#2236=LINE('',#12928,#3207);
#2237=LINE('',#12931,#3208);
#2238=LINE('',#12933,#3209);
#2239=LINE('',#12934,#3210);
#2240=LINE('',#12936,#3211);
#2241=LINE('',#12938,#3212);
#2242=LINE('',#12940,#3213);
#2243=LINE('',#12942,#3214);
#2244=LINE('',#12944,#3215);
#2245=LINE('',#12946,#3216);
#2246=LINE('',#12947,#3217);
#2247=LINE('',#12948,#3218);
#2248=LINE('',#12949,#3219);
#2249=LINE('',#12950,#3220);
#2250=LINE('',#12951,#3221);
#2251=LINE('',#12952,#3222);
#2252=LINE('',#12953,#3223);
#2253=LINE('',#12954,#3224);
#2254=LINE('',#12955,#3225);
#2255=LINE('',#12956,#3226);
#2256=LINE('',#12957,#3227);
#2257=LINE('',#12958,#3228);
#2258=LINE('',#12959,#3229);
#2259=LINE('',#12960,#3230);
#2260=LINE('',#12961,#3231);
#2261=LINE('',#12962,#3232);
#2262=LINE('',#12963,#3233);
#2263=LINE('',#12964,#3234);
#2264=LINE('',#12965,#3235);
#2265=LINE('',#12966,#3236);
#2266=LINE('',#12967,#3237);
#2267=LINE('',#12968,#3238);
#2268=LINE('',#12969,#3239);
#2269=LINE('',#12970,#3240);
#2270=LINE('',#12971,#3241);
#2271=LINE('',#12972,#3242);
#2272=LINE('',#12973,#3243);
#2273=LINE('',#12974,#3244);
#2274=LINE('',#12982,#3245);
#2275=LINE('',#12986,#3246);
#2276=LINE('',#12990,#3247);
#2277=LINE('',#12991,#3248);
#2278=LINE('',#12992,#3249);
#2279=LINE('',#12995,#3250);
#2280=LINE('',#12996,#3251);
#2281=LINE('',#12999,#3252);
#2282=LINE('',#13000,#3253);
#2283=LINE('',#13002,#3254);
#2284=LINE('',#13008,#3255);
#2285=LINE('',#13010,#3256);
#2286=LINE('',#13012,#3257);
#2287=LINE('',#13013,#3258);
#2288=LINE('',#13016,#3259);
#2289=LINE('',#13018,#3260);
#2290=LINE('',#13019,#3261);
#2291=LINE('',#13022,#3262);
#2292=LINE('',#13024,#3263);
#2293=LINE('',#13025,#3264);
#2294=LINE('',#13027,#3265);
#2295=LINE('',#13028,#3266);
#2296=LINE('',#13035,#3267);
#2297=LINE('',#13037,#3268);
#2298=LINE('',#13039,#3269);
#2299=LINE('',#13040,#3270);
#2300=LINE('',#13043,#3271);
#2301=LINE('',#13045,#3272);
#2302=LINE('',#13046,#3273);
#2303=LINE('',#13049,#3274);
#2304=LINE('',#13051,#3275);
#2305=LINE('',#13052,#3276);
#2306=LINE('',#13054,#3277);
#2307=LINE('',#13055,#3278);
#2308=LINE('',#13062,#3279);
#2309=LINE('',#13064,#3280);
#2310=LINE('',#13066,#3281);
#2311=LINE('',#13067,#3282);
#2312=LINE('',#13070,#3283);
#2313=LINE('',#13072,#3284);
#2314=LINE('',#13073,#3285);
#2315=LINE('',#13076,#3286);
#2316=LINE('',#13078,#3287);
#2317=LINE('',#13079,#3288);
#2318=LINE('',#13081,#3289);
#2319=LINE('',#13082,#3290);
#2320=LINE('',#13089,#3291);
#2321=LINE('',#13091,#3292);
#2322=LINE('',#13093,#3293);
#2323=LINE('',#13094,#3294);
#2324=LINE('',#13097,#3295);
#2325=LINE('',#13099,#3296);
#2326=LINE('',#13100,#3297);
#2327=LINE('',#13103,#3298);
#2328=LINE('',#13105,#3299);
#2329=LINE('',#13106,#3300);
#2330=LINE('',#13108,#3301);
#2331=LINE('',#13109,#3302);
#2332=LINE('',#13117,#3303);
#2333=LINE('',#13126,#3304);
#2334=LINE('',#13135,#3305);
#2335=LINE('',#13144,#3306);
#2336=LINE('',#13152,#3307);
#2337=LINE('',#13156,#3308);
#2338=LINE('',#13160,#3309);
#2339=LINE('',#13164,#3310);
#2340=LINE('',#13168,#3311);
#2341=LINE('',#13170,#3312);
#2342=LINE('',#13172,#3313);
#2343=LINE('',#13173,#3314);
#2344=LINE('',#13176,#3315);
#2345=LINE('',#13178,#3316);
#2346=LINE('',#13179,#3317);
#2347=LINE('',#13182,#3318);
#2348=LINE('',#13184,#3319);
#2349=LINE('',#13185,#3320);
#2350=LINE('',#13188,#3321);
#2351=LINE('',#13190,#3322);
#2352=LINE('',#13191,#3323);
#2353=LINE('',#13194,#3324);
#2354=LINE('',#13196,#3325);
#2355=LINE('',#13197,#3326);
#2356=LINE('',#13200,#3327);
#2357=LINE('',#13202,#3328);
#2358=LINE('',#13203,#3329);
#2359=LINE('',#13206,#3330);
#2360=LINE('',#13208,#3331);
#2361=LINE('',#13209,#3332);
#2362=LINE('',#13212,#3333);
#2363=LINE('',#13214,#3334);
#2364=LINE('',#13215,#3335);
#2365=LINE('',#13218,#3336);
#2366=LINE('',#13220,#3337);
#2367=LINE('',#13221,#3338);
#2368=LINE('',#13224,#3339);
#2369=LINE('',#13226,#3340);
#2370=LINE('',#13227,#3341);
#2371=LINE('',#13230,#3342);
#2372=LINE('',#13232,#3343);
#2373=LINE('',#13233,#3344);
#2374=LINE('',#13235,#3345);
#2375=LINE('',#13236,#3346);
#2376=LINE('',#13243,#3347);
#2377=LINE('',#13245,#3348);
#2378=LINE('',#13247,#3349);
#2379=LINE('',#13248,#3350);
#2380=LINE('',#13251,#3351);
#2381=LINE('',#13253,#3352);
#2382=LINE('',#13254,#3353);
#2383=LINE('',#13257,#3354);
#2384=LINE('',#13259,#3355);
#2385=LINE('',#13260,#3356);
#2386=LINE('',#13263,#3357);
#2387=LINE('',#13265,#3358);
#2388=LINE('',#13266,#3359);
#2389=LINE('',#13269,#3360);
#2390=LINE('',#13271,#3361);
#2391=LINE('',#13272,#3362);
#2392=LINE('',#13275,#3363);
#2393=LINE('',#13277,#3364);
#2394=LINE('',#13278,#3365);
#2395=LINE('',#13281,#3366);
#2396=LINE('',#13283,#3367);
#2397=LINE('',#13284,#3368);
#2398=LINE('',#13287,#3369);
#2399=LINE('',#13289,#3370);
#2400=LINE('',#13290,#3371);
#2401=LINE('',#13293,#3372);
#2402=LINE('',#13295,#3373);
#2403=LINE('',#13296,#3374);
#2404=LINE('',#13300,#3375);
#2405=LINE('',#13302,#3376);
#2406=LINE('',#13304,#3377);
#2407=LINE('',#13305,#3378);
#2408=LINE('',#13308,#3379);
#2409=LINE('',#13310,#3380);
#2410=LINE('',#13311,#3381);
#2411=LINE('',#13314,#3382);
#2412=LINE('',#13316,#3383);
#2413=LINE('',#13317,#3384);
#2414=LINE('',#13320,#3385);
#2415=LINE('',#13322,#3386);
#2416=LINE('',#13323,#3387);
#2417=LINE('',#13326,#3388);
#2418=LINE('',#13328,#3389);
#2419=LINE('',#13329,#3390);
#2420=LINE('',#13332,#3391);
#2421=LINE('',#13334,#3392);
#2422=LINE('',#13335,#3393);
#2423=LINE('',#13338,#3394);
#2424=LINE('',#13340,#3395);
#2425=LINE('',#13341,#3396);
#2426=LINE('',#13344,#3397);
#2427=LINE('',#13346,#3398);
#2428=LINE('',#13347,#3399);
#2429=LINE('',#13350,#3400);
#2430=LINE('',#13352,#3401);
#2431=LINE('',#13353,#3402);
#2432=LINE('',#13357,#3403);
#2433=LINE('',#13359,#3404);
#2434=LINE('',#13361,#3405);
#2435=LINE('',#13362,#3406);
#2436=LINE('',#13365,#3407);
#2437=LINE('',#13367,#3408);
#2438=LINE('',#13368,#3409);
#2439=LINE('',#13371,#3410);
#2440=LINE('',#13373,#3411);
#2441=LINE('',#13374,#3412);
#2442=LINE('',#13377,#3413);
#2443=LINE('',#13379,#3414);
#2444=LINE('',#13380,#3415);
#2445=LINE('',#13383,#3416);
#2446=LINE('',#13385,#3417);
#2447=LINE('',#13386,#3418);
#2448=LINE('',#13389,#3419);
#2449=LINE('',#13391,#3420);
#2450=LINE('',#13392,#3421);
#2451=LINE('',#13395,#3422);
#2452=LINE('',#13397,#3423);
#2453=LINE('',#13398,#3424);
#2454=LINE('',#13401,#3425);
#2455=LINE('',#13403,#3426);
#2456=LINE('',#13404,#3427);
#2457=LINE('',#13407,#3428);
#2458=LINE('',#13409,#3429);
#2459=LINE('',#13410,#3430);
#2460=LINE('',#13414,#3431);
#2461=LINE('',#13416,#3432);
#2462=LINE('',#13418,#3433);
#2463=LINE('',#13419,#3434);
#2464=LINE('',#13422,#3435);
#2465=LINE('',#13424,#3436);
#2466=LINE('',#13425,#3437);
#2467=LINE('',#13428,#3438);
#2468=LINE('',#13430,#3439);
#2469=LINE('',#13431,#3440);
#2470=LINE('',#13434,#3441);
#2471=LINE('',#13436,#3442);
#2472=LINE('',#13437,#3443);
#2473=LINE('',#13440,#3444);
#2474=LINE('',#13442,#3445);
#2475=LINE('',#13443,#3446);
#2476=LINE('',#13446,#3447);
#2477=LINE('',#13448,#3448);
#2478=LINE('',#13449,#3449);
#2479=LINE('',#13452,#3450);
#2480=LINE('',#13454,#3451);
#2481=LINE('',#13455,#3452);
#2482=LINE('',#13458,#3453);
#2483=LINE('',#13460,#3454);
#2484=LINE('',#13461,#3455);
#2485=LINE('',#13464,#3456);
#2486=LINE('',#13466,#3457);
#2487=LINE('',#13467,#3458);
#2488=LINE('',#13472,#3459);
#2489=LINE('',#13476,#3460);
#2490=LINE('',#13478,#3461);
#2491=LINE('',#13479,#3462);
#2492=LINE('',#13482,#3463);
#2493=LINE('',#13484,#3464);
#2494=LINE('',#13485,#3465);
#2495=LINE('',#13487,#3466);
#2496=LINE('',#13488,#3467);
#2497=LINE('',#13491,#3468);
#2498=LINE('',#13493,#3469);
#2499=LINE('',#13494,#3470);
#2500=LINE('',#13496,#3471);
#2501=LINE('',#13497,#3472);
#2502=LINE('',#13500,#3473);
#2503=LINE('',#13502,#3474);
#2504=LINE('',#13503,#3475);
#2505=LINE('',#13505,#3476);
#2506=LINE('',#13506,#3477);
#2507=LINE('',#13508,#3478);
#2508=LINE('',#13509,#3479);
#2509=LINE('',#13516,#3480);
#2510=LINE('',#13518,#3481);
#2511=LINE('',#13520,#3482);
#2512=LINE('',#13521,#3483);
#2513=LINE('',#13524,#3484);
#2514=LINE('',#13526,#3485);
#2515=LINE('',#13527,#3486);
#2516=LINE('',#13530,#3487);
#2517=LINE('',#13532,#3488);
#2518=LINE('',#13533,#3489);
#2519=LINE('',#13538,#3490);
#2520=LINE('',#13540,#3491);
#2521=LINE('',#13542,#3492);
#2522=LINE('',#13544,#3493);
#2523=LINE('',#13546,#3494);
#2524=LINE('',#13548,#3495);
#2525=LINE('',#13549,#3496);
#2526=LINE('',#13552,#3497);
#2527=LINE('',#13553,#3498);
#2528=LINE('',#13556,#3499);
#2529=LINE('',#13557,#3500);
#2530=LINE('',#13560,#3501);
#2531=LINE('',#13562,#3502);
#2532=LINE('',#13564,#3503);
#2533=LINE('',#13566,#3504);
#2534=LINE('',#13567,#3505);
#2535=LINE('',#13569,#3506);
#2536=LINE('',#13572,#3507);
#2537=LINE('',#13575,#3508);
#2538=LINE('',#13579,#3509);
#2539=LINE('',#13586,#3510);
#2540=LINE('',#13588,#3511);
#2541=LINE('',#13590,#3512);
#2542=LINE('',#13596,#3513);
#2543=LINE('',#13598,#3514);
#2544=LINE('',#13600,#3515);
#2545=LINE('',#13601,#3516);
#2546=LINE('',#13604,#3517);
#2547=LINE('',#13606,#3518);
#2548=LINE('',#13607,#3519);
#2549=LINE('',#13610,#3520);
#2550=LINE('',#13612,#3521);
#2551=LINE('',#13613,#3522);
#2552=LINE('',#13616,#3523);
#2553=LINE('',#13618,#3524);
#2554=LINE('',#13619,#3525);
#2555=LINE('',#13622,#3526);
#2556=LINE('',#13624,#3527);
#2557=LINE('',#13625,#3528);
#2558=LINE('',#13627,#3529);
#2559=LINE('',#13628,#3530);
#2560=LINE('',#13640,#3531);
#2561=LINE('',#13644,#3532);
#2562=LINE('',#13648,#3533);
#2563=LINE('',#13655,#3534);
#2564=LINE('',#13657,#3535);
#2565=LINE('',#13662,#3536);
#2566=LINE('',#13664,#3537);
#2567=LINE('',#13666,#3538);
#2568=LINE('',#13667,#3539);
#2569=LINE('',#13670,#3540);
#2570=LINE('',#13672,#3541);
#2571=LINE('',#13673,#3542);
#2572=LINE('',#13676,#3543);
#2573=LINE('',#13678,#3544);
#2574=LINE('',#13679,#3545);
#2575=LINE('',#13682,#3546);
#2576=LINE('',#13684,#3547);
#2577=LINE('',#13685,#3548);
#2578=LINE('',#13688,#3549);
#2579=LINE('',#13690,#3550);
#2580=LINE('',#13691,#3551);
#2581=LINE('',#13693,#3552);
#2582=LINE('',#13694,#3553);
#2583=LINE('',#13706,#3554);
#2584=LINE('',#13710,#3555);
#2585=LINE('',#13714,#3556);
#2586=LINE('',#13721,#3557);
#2587=LINE('',#13723,#3558);
#2588=LINE('',#13730,#3559);
#2589=LINE('',#13736,#3560);
#2590=LINE('',#13742,#3561);
#2591=LINE('',#13748,#3562);
#2592=LINE('',#13754,#3563);
#2593=LINE('',#13760,#3564);
#2594=LINE('',#13765,#3565);
#2595=LINE('',#13767,#3566);
#2596=LINE('',#13769,#3567);
#2597=LINE('',#13770,#3568);
#2598=LINE('',#13773,#3569);
#2599=LINE('',#13775,#3570);
#2600=LINE('',#13776,#3571);
#2601=LINE('',#13779,#3572);
#2602=LINE('',#13781,#3573);
#2603=LINE('',#13782,#3574);
#2604=LINE('',#13784,#3575);
#2605=LINE('',#13785,#3576);
#2606=LINE('',#13793,#3577);
#2607=LINE('',#13798,#3578);
#2608=LINE('',#13800,#3579);
#2609=LINE('',#13802,#3580);
#2610=LINE('',#13803,#3581);
#2611=LINE('',#13806,#3582);
#2612=LINE('',#13808,#3583);
#2613=LINE('',#13809,#3584);
#2614=LINE('',#13812,#3585);
#2615=LINE('',#13814,#3586);
#2616=LINE('',#13815,#3587);
#2617=LINE('',#13818,#3588);
#2618=LINE('',#13820,#3589);
#2619=LINE('',#13821,#3590);
#2620=LINE('',#13824,#3591);
#2621=LINE('',#13826,#3592);
#2622=LINE('',#13827,#3593);
#2623=LINE('',#13829,#3594);
#2624=LINE('',#13830,#3595);
#2625=LINE('',#13838,#3596);
#2626=LINE('',#13844,#3597);
#2627=LINE('',#13853,#3598);
#2628=LINE('',#13857,#3599);
#2629=LINE('',#13861,#3600);
#2630=LINE('',#13865,#3601);
#2631=LINE('',#13869,#3602);
#2632=LINE('',#13873,#3603);
#2633=LINE('',#13877,#3604);
#2634=LINE('',#13881,#3605);
#2635=LINE('',#13885,#3606);
#2636=LINE('',#13889,#3607);
#2637=LINE('',#13893,#3608);
#2638=LINE('',#13897,#3609);
#2639=LINE('',#13901,#3610);
#2640=LINE('',#13905,#3611);
#2641=LINE('',#13909,#3612);
#2642=LINE('',#13913,#3613);
#2643=LINE('',#13915,#3614);
#2644=LINE('',#13917,#3615);
#2645=LINE('',#13919,#3616);
#2646=LINE('',#13921,#3617);
#2647=LINE('',#13923,#3618);
#2648=LINE('',#13924,#3619);
#2649=LINE('',#13926,#3620);
#2650=LINE('',#13928,#3621);
#2651=LINE('',#13930,#3622);
#2652=LINE('',#13932,#3623);
#2653=LINE('',#13934,#3624);
#2654=LINE('',#13935,#3625);
#2655=LINE('',#13938,#3626);
#2656=LINE('',#13940,#3627);
#2657=LINE('',#13942,#3628);
#2658=LINE('',#13944,#3629);
#2659=LINE('',#13945,#3630);
#2660=LINE('',#13947,#3631);
#2661=LINE('',#13949,#3632);
#2662=LINE('',#13951,#3633);
#2663=LINE('',#13953,#3634);
#2664=LINE('',#13954,#3635);
#2665=LINE('',#13957,#3636);
#2666=LINE('',#13958,#3637);
#2667=LINE('',#13961,#3638);
#2668=LINE('',#13962,#3639);
#2669=LINE('',#13965,#3640);
#2670=LINE('',#13966,#3641);
#2671=LINE('',#13969,#3642);
#2672=LINE('',#13970,#3643);
#2673=LINE('',#13972,#3644);
#2674=LINE('',#13975,#3645);
#2675=LINE('',#13976,#3646);
#2676=LINE('',#13979,#3647);
#2677=LINE('',#13980,#3648);
#2678=LINE('',#13983,#3649);
#2679=LINE('',#13984,#3650);
#2680=LINE('',#13987,#3651);
#2681=LINE('',#13988,#3652);
#2682=LINE('',#13990,#3653);
#2683=LINE('',#13996,#3654);
#2684=LINE('',#13998,#3655);
#2685=LINE('',#14000,#3656);
#2686=LINE('',#14001,#3657);
#2687=LINE('',#14004,#3658);
#2688=LINE('',#14006,#3659);
#2689=LINE('',#14007,#3660);
#2690=LINE('',#14010,#3661);
#2691=LINE('',#14012,#3662);
#2692=LINE('',#14013,#3663);
#2693=LINE('',#14016,#3664);
#2694=LINE('',#14018,#3665);
#2695=LINE('',#14019,#3666);
#2696=LINE('',#14022,#3667);
#2697=LINE('',#14024,#3668);
#2698=LINE('',#14025,#3669);
#2699=LINE('',#14028,#3670);
#2700=LINE('',#14030,#3671);
#2701=LINE('',#14031,#3672);
#2702=LINE('',#14034,#3673);
#2703=LINE('',#14036,#3674);
#2704=LINE('',#14037,#3675);
#2705=LINE('',#14039,#3676);
#2706=LINE('',#14040,#3677);
#2707=LINE('',#14047,#3678);
#2708=LINE('',#14049,#3679);
#2709=LINE('',#14051,#3680);
#2710=LINE('',#14052,#3681);
#2711=LINE('',#14055,#3682);
#2712=LINE('',#14057,#3683);
#2713=LINE('',#14058,#3684);
#2714=LINE('',#14061,#3685);
#2715=LINE('',#14063,#3686);
#2716=LINE('',#14064,#3687);
#2717=LINE('',#14067,#3688);
#2718=LINE('',#14069,#3689);
#2719=LINE('',#14070,#3690);
#2720=LINE('',#14073,#3691);
#2721=LINE('',#14075,#3692);
#2722=LINE('',#14076,#3693);
#2723=LINE('',#14079,#3694);
#2724=LINE('',#14081,#3695);
#2725=LINE('',#14082,#3696);
#2726=LINE('',#14085,#3697);
#2727=LINE('',#14087,#3698);
#2728=LINE('',#14088,#3699);
#2729=LINE('',#14090,#3700);
#2730=LINE('',#14091,#3701);
#2731=LINE('',#14102,#3702);
#2732=LINE('',#14106,#3703);
#2733=LINE('',#14113,#3704);
#2734=LINE('',#14123,#3705);
#2735=LINE('',#14127,#3706);
#2736=LINE('',#14131,#3707);
#2737=LINE('',#14138,#3708);
#2738=LINE('',#14142,#3709);
#2739=LINE('',#14146,#3710);
#2740=LINE('',#14151,#3711);
#2741=LINE('',#14153,#3712);
#2742=LINE('',#14155,#3713);
#2743=LINE('',#14156,#3714);
#2744=LINE('',#14159,#3715);
#2745=LINE('',#14161,#3716);
#2746=LINE('',#14162,#3717);
#2747=LINE('',#14165,#3718);
#2748=LINE('',#14167,#3719);
#2749=LINE('',#14168,#3720);
#2750=LINE('',#14171,#3721);
#2751=LINE('',#14173,#3722);
#2752=LINE('',#14174,#3723);
#2753=LINE('',#14177,#3724);
#2754=LINE('',#14179,#3725);
#2755=LINE('',#14180,#3726);
#2756=LINE('',#14182,#3727);
#2757=LINE('',#14183,#3728);
#2758=LINE('',#14191,#3729);
#2759=LINE('',#14195,#3730);
#2760=LINE('',#14202,#3731);
#2761=LINE('',#14212,#3732);
#2762=LINE('',#14216,#3733);
#2763=LINE('',#14220,#3734);
#2764=LINE('',#14227,#3735);
#2765=LINE('',#14231,#3736);
#2766=LINE('',#14235,#3737);
#2767=LINE('',#14240,#3738);
#2768=LINE('',#14242,#3739);
#2769=LINE('',#14244,#3740);
#2770=LINE('',#14245,#3741);
#2771=LINE('',#14248,#3742);
#2772=LINE('',#14250,#3743);
#2773=LINE('',#14251,#3744);
#2774=LINE('',#14254,#3745);
#2775=LINE('',#14256,#3746);
#2776=LINE('',#14257,#3747);
#2777=LINE('',#14260,#3748);
#2778=LINE('',#14262,#3749);
#2779=LINE('',#14263,#3750);
#2780=LINE('',#14266,#3751);
#2781=LINE('',#14268,#3752);
#2782=LINE('',#14269,#3753);
#2783=LINE('',#14271,#3754);
#2784=LINE('',#14272,#3755);
#2785=LINE('',#14317,#3756);
#2786=LINE('',#14323,#3757);
#2787=LINE('',#14334,#3758);
#2788=LINE('',#14338,#3759);
#2789=LINE('',#14342,#3760);
#2790=LINE('',#14349,#3761);
#2791=LINE('',#14353,#3762);
#2792=LINE('',#14357,#3763);
#2793=LINE('',#14362,#3764);
#2794=LINE('',#14364,#3765);
#2795=LINE('',#14366,#3766);
#2796=LINE('',#14367,#3767);
#2797=LINE('',#14370,#3768);
#2798=LINE('',#14372,#3769);
#2799=LINE('',#14373,#3770);
#2800=LINE('',#14376,#3771);
#2801=LINE('',#14378,#3772);
#2802=LINE('',#14379,#3773);
#2803=LINE('',#14382,#3774);
#2804=LINE('',#14384,#3775);
#2805=LINE('',#14385,#3776);
#2806=LINE('',#14388,#3777);
#2807=LINE('',#14390,#3778);
#2808=LINE('',#14391,#3779);
#2809=LINE('',#14393,#3780);
#2810=LINE('',#14394,#3781);
#2811=VECTOR('',#9631,0.165);
#2812=VECTOR('',#9638,0.164999999999999);
#2813=VECTOR('',#9645,0.210000000000001);
#2814=VECTOR('',#9652,0.21);
#2815=VECTOR('',#9659,0.21);
#2816=VECTOR('',#9666,0.210000000000001);
#2817=VECTOR('',#9673,0.274999999999999);
#2818=VECTOR('',#9680,0.275);
#2819=VECTOR('',#9687,0.275);
#2820=VECTOR('',#9694,0.274999999999999);
#2821=VECTOR('',#9701,0.164999999999999);
#2822=VECTOR('',#9708,0.164999999999999);
#2823=VECTOR('',#9715,0.165);
#2824=VECTOR('',#9722,0.164999999999999);
#2825=VECTOR('',#9727,1.);
#2826=VECTOR('',#9728,1.);
#2827=VECTOR('',#9729,1.);
#2828=VECTOR('',#9730,1.);
#2829=VECTOR('',#9733,1.);
#2830=VECTOR('',#9734,1.);
#2831=VECTOR('',#9735,1.);
#2832=VECTOR('',#9738,1.);
#2833=VECTOR('',#9739,1.);
#2834=VECTOR('',#9740,1.);
#2835=VECTOR('',#9743,1.);
#2836=VECTOR('',#9744,1.);
#2837=VECTOR('',#9755,0.475);
#2838=VECTOR('',#9766,0.475);
#2839=VECTOR('',#9777,0.275);
#2840=VECTOR('',#9782,0.275);
#2841=VECTOR('',#9785,1.);
#2842=VECTOR('',#9786,1.);
#2843=VECTOR('',#9787,1.);
#2844=VECTOR('',#9788,1.);
#2845=VECTOR('',#9791,1.);
#2846=VECTOR('',#9792,1.);
#2847=VECTOR('',#9793,1.);
#2848=VECTOR('',#9796,1.);
#2849=VECTOR('',#9797,1.);
#2850=VECTOR('',#9798,1.);
#2851=VECTOR('',#9801,1.);
#2852=VECTOR('',#9802,1.);
#2853=VECTOR('',#9811,1.);
#2854=VECTOR('',#9812,1.);
#2855=VECTOR('',#9813,1.);
#2856=VECTOR('',#9814,1.);
#2857=VECTOR('',#9817,1.);
#2858=VECTOR('',#9818,1.);
#2859=VECTOR('',#9819,1.);
#2860=VECTOR('',#9822,1.);
#2861=VECTOR('',#9823,1.);
#2862=VECTOR('',#9824,1.);
#2863=VECTOR('',#9827,1.);
#2864=VECTOR('',#9828,1.);
#2865=VECTOR('',#9839,0.475000000000001);
#2866=VECTOR('',#9850,0.475000000000001);
#2867=VECTOR('',#9861,0.274999999999999);
#2868=VECTOR('',#9866,0.274999999999999);
#2869=VECTOR('',#9869,1.);
#2870=VECTOR('',#9870,1.);
#2871=VECTOR('',#9871,1.);
#2872=VECTOR('',#9872,1.);
#2873=VECTOR('',#9875,1.);
#2874=VECTOR('',#9876,1.);
#2875=VECTOR('',#9877,1.);
#2876=VECTOR('',#9880,1.);
#2877=VECTOR('',#9881,1.);
#2878=VECTOR('',#9882,1.);
#2879=VECTOR('',#9885,1.);
#2880=VECTOR('',#9886,1.);
#2881=VECTOR('',#9895,1.);
#2882=VECTOR('',#9896,1.);
#2883=VECTOR('',#9897,1.);
#2884=VECTOR('',#9898,1.);
#2885=VECTOR('',#9901,1.);
#2886=VECTOR('',#9902,1.);
#2887=VECTOR('',#9903,1.);
#2888=VECTOR('',#9906,1.);
#2889=VECTOR('',#9907,1.);
#2890=VECTOR('',#9908,1.);
#2891=VECTOR('',#9911,1.);
#2892=VECTOR('',#9912,1.);
#2893=VECTOR('',#9921,1.);
#2894=VECTOR('',#9922,1.);
#2895=VECTOR('',#9923,1.);
#2896=VECTOR('',#9924,1.);
#2897=VECTOR('',#9927,1.);
#2898=VECTOR('',#9928,1.);
#2899=VECTOR('',#9929,1.);
#2900=VECTOR('',#9932,1.);
#2901=VECTOR('',#9933,1.);
#2902=VECTOR('',#9934,1.);
#2903=VECTOR('',#9937,1.);
#2904=VECTOR('',#9940,1.);
#2905=VECTOR('',#9941,1.);
#2906=VECTOR('',#9942,1.);
#2907=VECTOR('',#9943,1.);
#2908=VECTOR('',#9946,1.);
#2909=VECTOR('',#9947,1.);
#2910=VECTOR('',#9948,1.);
#2911=VECTOR('',#9951,1.);
#2912=VECTOR('',#9952,1.);
#2913=VECTOR('',#9953,1.);
#2914=VECTOR('',#9956,1.);
#2915=VECTOR('',#9959,1.);
#2916=VECTOR('',#9960,1.);
#2917=VECTOR('',#9961,1.);
#2918=VECTOR('',#9962,1.);
#2919=VECTOR('',#9965,1.);
#2920=VECTOR('',#9966,1.);
#2921=VECTOR('',#9967,1.);
#2922=VECTOR('',#9970,1.);
#2923=VECTOR('',#9971,1.);
#2924=VECTOR('',#9972,1.);
#2925=VECTOR('',#9975,1.);
#2926=VECTOR('',#9978,1.);
#2927=VECTOR('',#9979,1.);
#2928=VECTOR('',#9980,1.);
#2929=VECTOR('',#9981,1.);
#2930=VECTOR('',#9984,1.);
#2931=VECTOR('',#9985,1.);
#2932=VECTOR('',#9986,1.);
#2933=VECTOR('',#9989,1.);
#2934=VECTOR('',#9990,1.);
#2935=VECTOR('',#9991,1.);
#2936=VECTOR('',#9994,1.);
#2937=VECTOR('',#9997,1.);
#2938=VECTOR('',#9998,1.);
#2939=VECTOR('',#9999,1.);
#2940=VECTOR('',#10000,1.);
#2941=VECTOR('',#10003,1.);
#2942=VECTOR('',#10004,1.);
#2943=VECTOR('',#10005,1.);
#2944=VECTOR('',#10008,1.);
#2945=VECTOR('',#10009,1.);
#2946=VECTOR('',#10010,1.);
#2947=VECTOR('',#10013,1.);
#2948=VECTOR('',#10016,1.);
#2949=VECTOR('',#10017,1.);
#2950=VECTOR('',#10018,1.);
#2951=VECTOR('',#10019,1.);
#2952=VECTOR('',#10022,1.);
#2953=VECTOR('',#10023,1.);
#2954=VECTOR('',#10024,1.);
#2955=VECTOR('',#10027,1.);
#2956=VECTOR('',#10028,1.);
#2957=VECTOR('',#10029,1.);
#2958=VECTOR('',#10032,1.);
#2959=VECTOR('',#10035,1.);
#2960=VECTOR('',#10036,1.);
#2961=VECTOR('',#10037,1.);
#2962=VECTOR('',#10038,1.);
#2963=VECTOR('',#10041,1.);
#2964=VECTOR('',#10042,1.);
#2965=VECTOR('',#10043,1.);
#2966=VECTOR('',#10046,1.);
#2967=VECTOR('',#10047,1.);
#2968=VECTOR('',#10048,1.);
#2969=VECTOR('',#10051,1.);
#2970=VECTOR('',#10054,1.);
#2971=VECTOR('',#10055,1.);
#2972=VECTOR('',#10056,1.);
#2973=VECTOR('',#10057,1.);
#2974=VECTOR('',#10060,1.);
#2975=VECTOR('',#10061,1.);
#2976=VECTOR('',#10062,1.);
#2977=VECTOR('',#10065,1.);
#2978=VECTOR('',#10066,1.);
#2979=VECTOR('',#10067,1.);
#2980=VECTOR('',#10070,1.);
#2981=VECTOR('',#10073,1.);
#2982=VECTOR('',#10074,1.);
#2983=VECTOR('',#10075,1.);
#2984=VECTOR('',#10076,1.);
#2985=VECTOR('',#10079,1.);
#2986=VECTOR('',#10080,1.);
#2987=VECTOR('',#10081,1.);
#2988=VECTOR('',#10084,1.);
#2989=VECTOR('',#10085,1.);
#2990=VECTOR('',#10086,1.);
#2991=VECTOR('',#10089,1.);
#2992=VECTOR('',#10092,1.);
#2993=VECTOR('',#10093,1.);
#2994=VECTOR('',#10094,1.);
#2995=VECTOR('',#10095,1.);
#2996=VECTOR('',#10098,1.);
#2997=VECTOR('',#10099,1.);
#2998=VECTOR('',#10100,1.);
#2999=VECTOR('',#10103,1.);
#3000=VECTOR('',#10104,1.);
#3001=VECTOR('',#10105,1.);
#3002=VECTOR('',#10108,1.);
#3003=VECTOR('',#10111,1.);
#3004=VECTOR('',#10112,1.);
#3005=VECTOR('',#10113,1.);
#3006=VECTOR('',#10114,1.);
#3007=VECTOR('',#10117,1.);
#3008=VECTOR('',#10118,1.);
#3009=VECTOR('',#10119,1.);
#3010=VECTOR('',#10122,1.);
#3011=VECTOR('',#10123,1.);
#3012=VECTOR('',#10124,1.);
#3013=VECTOR('',#10127,1.);
#3014=VECTOR('',#10130,1.);
#3015=VECTOR('',#10131,1.);
#3016=VECTOR('',#10132,1.);
#3017=VECTOR('',#10133,1.);
#3018=VECTOR('',#10136,1.);
#3019=VECTOR('',#10137,1.);
#3020=VECTOR('',#10138,1.);
#3021=VECTOR('',#10141,1.);
#3022=VECTOR('',#10142,1.);
#3023=VECTOR('',#10143,1.);
#3024=VECTOR('',#10146,1.);
#3025=VECTOR('',#10149,1.);
#3026=VECTOR('',#10150,1.);
#3027=VECTOR('',#10151,1.);
#3028=VECTOR('',#10152,1.);
#3029=VECTOR('',#10155,1.);
#3030=VECTOR('',#10156,1.);
#3031=VECTOR('',#10157,1.);
#3032=VECTOR('',#10160,1.);
#3033=VECTOR('',#10161,1.);
#3034=VECTOR('',#10162,1.);
#3035=VECTOR('',#10165,1.);
#3036=VECTOR('',#10168,1.);
#3037=VECTOR('',#10169,1.);
#3038=VECTOR('',#10170,1.);
#3039=VECTOR('',#10171,1.);
#3040=VECTOR('',#10174,1.);
#3041=VECTOR('',#10175,1.);
#3042=VECTOR('',#10176,1.);
#3043=VECTOR('',#10179,1.);
#3044=VECTOR('',#10180,1.);
#3045=VECTOR('',#10181,1.);
#3046=VECTOR('',#10184,1.);
#3047=VECTOR('',#10187,1.);
#3048=VECTOR('',#10188,1.);
#3049=VECTOR('',#10189,1.);
#3050=VECTOR('',#10190,1.);
#3051=VECTOR('',#10193,1.);
#3052=VECTOR('',#10194,1.);
#3053=VECTOR('',#10195,1.);
#3054=VECTOR('',#10198,1.);
#3055=VECTOR('',#10199,1.);
#3056=VECTOR('',#10200,1.);
#3057=VECTOR('',#10203,1.);
#3058=VECTOR('',#10206,1.);
#3059=VECTOR('',#10207,1.);
#3060=VECTOR('',#10208,1.);
#3061=VECTOR('',#10209,1.);
#3062=VECTOR('',#10212,1.);
#3063=VECTOR('',#10213,1.);
#3064=VECTOR('',#10214,1.);
#3065=VECTOR('',#10217,1.);
#3066=VECTOR('',#10218,1.);
#3067=VECTOR('',#10219,1.);
#3068=VECTOR('',#10222,1.);
#3069=VECTOR('',#10225,1.);
#3070=VECTOR('',#10226,1.);
#3071=VECTOR('',#10227,1.);
#3072=VECTOR('',#10228,1.);
#3073=VECTOR('',#10231,1.);
#3074=VECTOR('',#10232,1.);
#3075=VECTOR('',#10233,1.);
#3076=VECTOR('',#10236,1.);
#3077=VECTOR('',#10237,1.);
#3078=VECTOR('',#10238,1.);
#3079=VECTOR('',#10241,1.);
#3080=VECTOR('',#10244,1.);
#3081=VECTOR('',#10245,1.);
#3082=VECTOR('',#10246,1.);
#3083=VECTOR('',#10247,1.);
#3084=VECTOR('',#10250,1.);
#3085=VECTOR('',#10251,1.);
#3086=VECTOR('',#10252,1.);
#3087=VECTOR('',#10255,1.);
#3088=VECTOR('',#10256,1.);
#3089=VECTOR('',#10257,1.);
#3090=VECTOR('',#10260,1.);
#3091=VECTOR('',#10263,1.);
#3092=VECTOR('',#10264,1.);
#3093=VECTOR('',#10265,1.);
#3094=VECTOR('',#10266,1.);
#3095=VECTOR('',#10269,1.);
#3096=VECTOR('',#10270,1.);
#3097=VECTOR('',#10271,1.);
#3098=VECTOR('',#10274,1.);
#3099=VECTOR('',#10275,1.);
#3100=VECTOR('',#10276,1.);
#3101=VECTOR('',#10279,1.);
#3102=VECTOR('',#10282,1.);
#3103=VECTOR('',#10283,1.);
#3104=VECTOR('',#10284,1.);
#3105=VECTOR('',#10285,1.);
#3106=VECTOR('',#10288,1.);
#3107=VECTOR('',#10289,1.);
#3108=VECTOR('',#10290,1.);
#3109=VECTOR('',#10293,1.);
#3110=VECTOR('',#10294,1.);
#3111=VECTOR('',#10295,1.);
#3112=VECTOR('',#10298,1.);
#3113=VECTOR('',#10301,1.);
#3114=VECTOR('',#10302,1.);
#3115=VECTOR('',#10303,1.);
#3116=VECTOR('',#10304,1.);
#3117=VECTOR('',#10307,1.);
#3118=VECTOR('',#10308,1.);
#3119=VECTOR('',#10309,1.);
#3120=VECTOR('',#10312,1.);
#3121=VECTOR('',#10313,1.);
#3122=VECTOR('',#10314,1.);
#3123=VECTOR('',#10317,1.);
#3124=VECTOR('',#10320,1.);
#3125=VECTOR('',#10321,1.);
#3126=VECTOR('',#10322,1.);
#3127=VECTOR('',#10323,1.);
#3128=VECTOR('',#10326,1.);
#3129=VECTOR('',#10327,1.);
#3130=VECTOR('',#10328,1.);
#3131=VECTOR('',#10331,1.);
#3132=VECTOR('',#10332,1.);
#3133=VECTOR('',#10333,1.);
#3134=VECTOR('',#10336,1.);
#3135=VECTOR('',#10339,1.);
#3136=VECTOR('',#10340,1.);
#3137=VECTOR('',#10341,1.);
#3138=VECTOR('',#10342,1.);
#3139=VECTOR('',#10345,1.);
#3140=VECTOR('',#10346,1.);
#3141=VECTOR('',#10347,1.);
#3142=VECTOR('',#10350,1.);
#3143=VECTOR('',#10351,1.);
#3144=VECTOR('',#10352,1.);
#3145=VECTOR('',#10355,1.);
#3146=VECTOR('',#10358,1.);
#3147=VECTOR('',#10359,1.);
#3148=VECTOR('',#10360,1.);
#3149=VECTOR('',#10361,1.);
#3150=VECTOR('',#10364,1.);
#3151=VECTOR('',#10365,1.);
#3152=VECTOR('',#10366,1.);
#3153=VECTOR('',#10369,1.);
#3154=VECTOR('',#10370,1.);
#3155=VECTOR('',#10371,1.);
#3156=VECTOR('',#10374,1.);
#3157=VECTOR('',#10377,1.);
#3158=VECTOR('',#10378,1.);
#3159=VECTOR('',#10379,1.);
#3160=VECTOR('',#10380,1.);
#3161=VECTOR('',#10383,1.);
#3162=VECTOR('',#10384,1.);
#3163=VECTOR('',#10385,1.);
#3164=VECTOR('',#10388,1.);
#3165=VECTOR('',#10389,1.);
#3166=VECTOR('',#10390,1.);
#3167=VECTOR('',#10393,1.);
#3168=VECTOR('',#10396,1.);
#3169=VECTOR('',#10397,1.);
#3170=VECTOR('',#10398,1.);
#3171=VECTOR('',#10399,1.);
#3172=VECTOR('',#10402,1.);
#3173=VECTOR('',#10403,1.);
#3174=VECTOR('',#10404,1.);
#3175=VECTOR('',#10407,1.);
#3176=VECTOR('',#10408,1.);
#3177=VECTOR('',#10409,1.);
#3178=VECTOR('',#10412,1.);
#3179=VECTOR('',#10415,1.);
#3180=VECTOR('',#10416,1.);
#3181=VECTOR('',#10417,1.);
#3182=VECTOR('',#10418,1.);
#3183=VECTOR('',#10421,1.);
#3184=VECTOR('',#10422,1.);
#3185=VECTOR('',#10423,1.);
#3186=VECTOR('',#10426,1.);
#3187=VECTOR('',#10427,1.);
#3188=VECTOR('',#10428,1.);
#3189=VECTOR('',#10431,1.);
#3190=VECTOR('',#10434,1.);
#3191=VECTOR('',#10435,1.);
#3192=VECTOR('',#10436,1.);
#3193=VECTOR('',#10437,1.);
#3194=VECTOR('',#10440,1.);
#3195=VECTOR('',#10441,1.);
#3196=VECTOR('',#10442,1.);
#3197=VECTOR('',#10445,1.);
#3198=VECTOR('',#10446,1.);
#3199=VECTOR('',#10447,1.);
#3200=VECTOR('',#10450,1.);
#3201=VECTOR('',#10453,1.);
#3202=VECTOR('',#10454,1.);
#3203=VECTOR('',#10455,1.);
#3204=VECTOR('',#10456,1.);
#3205=VECTOR('',#10459,1.);
#3206=VECTOR('',#10460,1.);
#3207=VECTOR('',#10461,1.);
#3208=VECTOR('',#10464,1.);
#3209=VECTOR('',#10465,1.);
#3210=VECTOR('',#10466,1.);
#3211=VECTOR('',#10469,1.);
#3212=VECTOR('',#10472,1.);
#3213=VECTOR('',#10473,1.);
#3214=VECTOR('',#10474,1.);
#3215=VECTOR('',#10475,1.);
#3216=VECTOR('',#10476,1.);
#3217=VECTOR('',#10477,1.);
#3218=VECTOR('',#10478,1.);
#3219=VECTOR('',#10479,1.);
#3220=VECTOR('',#10480,1.);
#3221=VECTOR('',#10481,1.);
#3222=VECTOR('',#10482,1.);
#3223=VECTOR('',#10483,1.);
#3224=VECTOR('',#10484,1.);
#3225=VECTOR('',#10485,1.);
#3226=VECTOR('',#10486,1.);
#3227=VECTOR('',#10487,1.);
#3228=VECTOR('',#10488,1.);
#3229=VECTOR('',#10489,1.);
#3230=VECTOR('',#10490,1.);
#3231=VECTOR('',#10491,1.);
#3232=VECTOR('',#10492,1.);
#3233=VECTOR('',#10493,1.);
#3234=VECTOR('',#10494,1.);
#3235=VECTOR('',#10495,1.);
#3236=VECTOR('',#10496,1.);
#3237=VECTOR('',#10497,1.);
#3238=VECTOR('',#10498,1.);
#3239=VECTOR('',#10499,1.);
#3240=VECTOR('',#10500,1.);
#3241=VECTOR('',#10501,1.);
#3242=VECTOR('',#10502,1.);
#3243=VECTOR('',#10503,1.);
#3244=VECTOR('',#10504,1.);
#3245=VECTOR('',#10513,0.225);
#3246=VECTOR('',#10518,0.225000000000001);
#3247=VECTOR('',#10521,1.);
#3248=VECTOR('',#10522,1.);
#3249=VECTOR('',#10523,1.);
#3250=VECTOR('',#10526,1.);
#3251=VECTOR('',#10527,1.);
#3252=VECTOR('',#10530,1.);
#3253=VECTOR('',#10531,1.);
#3254=VECTOR('',#10534,1.);
#3255=VECTOR('',#10541,1.);
#3256=VECTOR('',#10542,1.);
#3257=VECTOR('',#10543,1.);
#3258=VECTOR('',#10544,1.);
#3259=VECTOR('',#10547,1.);
#3260=VECTOR('',#10548,1.);
#3261=VECTOR('',#10549,1.);
#3262=VECTOR('',#10552,1.);
#3263=VECTOR('',#10553,1.);
#3264=VECTOR('',#10554,1.);
#3265=VECTOR('',#10557,1.);
#3266=VECTOR('',#10558,1.);
#3267=VECTOR('',#10567,1.);
#3268=VECTOR('',#10568,1.);
#3269=VECTOR('',#10569,1.);
#3270=VECTOR('',#10570,1.);
#3271=VECTOR('',#10573,1.);
#3272=VECTOR('',#10574,1.);
#3273=VECTOR('',#10575,1.);
#3274=VECTOR('',#10578,1.);
#3275=VECTOR('',#10579,1.);
#3276=VECTOR('',#10580,1.);
#3277=VECTOR('',#10583,1.);
#3278=VECTOR('',#10584,1.);
#3279=VECTOR('',#10593,1.);
#3280=VECTOR('',#10594,1.);
#3281=VECTOR('',#10595,1.);
#3282=VECTOR('',#10596,1.);
#3283=VECTOR('',#10599,1.);
#3284=VECTOR('',#10600,1.);
#3285=VECTOR('',#10601,1.);
#3286=VECTOR('',#10604,1.);
#3287=VECTOR('',#10605,1.);
#3288=VECTOR('',#10606,1.);
#3289=VECTOR('',#10609,1.);
#3290=VECTOR('',#10610,1.);
#3291=VECTOR('',#10619,1.);
#3292=VECTOR('',#10620,1.);
#3293=VECTOR('',#10621,1.);
#3294=VECTOR('',#10622,1.);
#3295=VECTOR('',#10625,1.);
#3296=VECTOR('',#10626,1.);
#3297=VECTOR('',#10627,1.);
#3298=VECTOR('',#10630,1.);
#3299=VECTOR('',#10631,1.);
#3300=VECTOR('',#10632,1.);
#3301=VECTOR('',#10635,1.);
#3302=VECTOR('',#10636,1.);
#3303=VECTOR('',#10647,0.375);
#3304=VECTOR('',#10658,0.375);
#3305=VECTOR('',#10669,0.375);
#3306=VECTOR('',#10680,0.375);
#3307=VECTOR('',#10691,0.225);
#3308=VECTOR('',#10696,0.225);
#3309=VECTOR('',#10701,0.225);
#3310=VECTOR('',#10706,0.225000000000001);
#3311=VECTOR('',#10709,1.);
#3312=VECTOR('',#10710,1.);
#3313=VECTOR('',#10711,1.);
#3314=VECTOR('',#10712,1.);
#3315=VECTOR('',#10715,1.);
#3316=VECTOR('',#10716,1.);
#3317=VECTOR('',#10717,1.);
#3318=VECTOR('',#10720,1.);
#3319=VECTOR('',#10721,1.);
#3320=VECTOR('',#10722,1.);
#3321=VECTOR('',#10725,1.);
#3322=VECTOR('',#10726,1.);
#3323=VECTOR('',#10727,1.);
#3324=VECTOR('',#10730,1.);
#3325=VECTOR('',#10731,1.);
#3326=VECTOR('',#10732,1.);
#3327=VECTOR('',#10735,1.);
#3328=VECTOR('',#10736,1.);
#3329=VECTOR('',#10737,1.);
#3330=VECTOR('',#10740,1.);
#3331=VECTOR('',#10741,1.);
#3332=VECTOR('',#10742,1.);
#3333=VECTOR('',#10745,1.);
#3334=VECTOR('',#10746,1.);
#3335=VECTOR('',#10747,1.);
#3336=VECTOR('',#10750,1.);
#3337=VECTOR('',#10751,1.);
#3338=VECTOR('',#10752,1.);
#3339=VECTOR('',#10755,1.);
#3340=VECTOR('',#10756,1.);
#3341=VECTOR('',#10757,1.);
#3342=VECTOR('',#10760,1.);
#3343=VECTOR('',#10761,1.);
#3344=VECTOR('',#10762,1.);
#3345=VECTOR('',#10765,1.);
#3346=VECTOR('',#10766,1.);
#3347=VECTOR('',#10775,1.);
#3348=VECTOR('',#10776,1.);
#3349=VECTOR('',#10777,1.);
#3350=VECTOR('',#10778,1.);
#3351=VECTOR('',#10781,1.);
#3352=VECTOR('',#10782,1.);
#3353=VECTOR('',#10783,1.);
#3354=VECTOR('',#10786,1.);
#3355=VECTOR('',#10787,1.);
#3356=VECTOR('',#10788,1.);
#3357=VECTOR('',#10791,1.);
#3358=VECTOR('',#10792,1.);
#3359=VECTOR('',#10793,1.);
#3360=VECTOR('',#10796,1.);
#3361=VECTOR('',#10797,1.);
#3362=VECTOR('',#10798,1.);
#3363=VECTOR('',#10801,1.);
#3364=VECTOR('',#10802,1.);
#3365=VECTOR('',#10803,1.);
#3366=VECTOR('',#10806,1.);
#3367=VECTOR('',#10807,1.);
#3368=VECTOR('',#10808,1.);
#3369=VECTOR('',#10811,1.);
#3370=VECTOR('',#10812,1.);
#3371=VECTOR('',#10813,1.);
#3372=VECTOR('',#10816,1.);
#3373=VECTOR('',#10817,1.);
#3374=VECTOR('',#10818,1.);
#3375=VECTOR('',#10821,1.);
#3376=VECTOR('',#10822,1.);
#3377=VECTOR('',#10823,1.);
#3378=VECTOR('',#10824,1.);
#3379=VECTOR('',#10827,1.);
#3380=VECTOR('',#10828,1.);
#3381=VECTOR('',#10829,1.);
#3382=VECTOR('',#10832,1.);
#3383=VECTOR('',#10833,1.);
#3384=VECTOR('',#10834,1.);
#3385=VECTOR('',#10837,1.);
#3386=VECTOR('',#10838,1.);
#3387=VECTOR('',#10839,1.);
#3388=VECTOR('',#10842,1.);
#3389=VECTOR('',#10843,1.);
#3390=VECTOR('',#10844,1.);
#3391=VECTOR('',#10847,1.);
#3392=VECTOR('',#10848,1.);
#3393=VECTOR('',#10849,1.);
#3394=VECTOR('',#10852,1.);
#3395=VECTOR('',#10853,1.);
#3396=VECTOR('',#10854,1.);
#3397=VECTOR('',#10857,1.);
#3398=VECTOR('',#10858,1.);
#3399=VECTOR('',#10859,1.);
#3400=VECTOR('',#10862,1.);
#3401=VECTOR('',#10863,1.);
#3402=VECTOR('',#10864,1.);
#3403=VECTOR('',#10867,1.);
#3404=VECTOR('',#10868,1.);
#3405=VECTOR('',#10869,1.);
#3406=VECTOR('',#10870,1.);
#3407=VECTOR('',#10873,1.);
#3408=VECTOR('',#10874,1.);
#3409=VECTOR('',#10875,1.);
#3410=VECTOR('',#10878,1.);
#3411=VECTOR('',#10879,1.);
#3412=VECTOR('',#10880,1.);
#3413=VECTOR('',#10883,1.);
#3414=VECTOR('',#10884,1.);
#3415=VECTOR('',#10885,1.);
#3416=VECTOR('',#10888,1.);
#3417=VECTOR('',#10889,1.);
#3418=VECTOR('',#10890,1.);
#3419=VECTOR('',#10893,1.);
#3420=VECTOR('',#10894,1.);
#3421=VECTOR('',#10895,1.);
#3422=VECTOR('',#10898,1.);
#3423=VECTOR('',#10899,1.);
#3424=VECTOR('',#10900,1.);
#3425=VECTOR('',#10903,1.);
#3426=VECTOR('',#10904,1.);
#3427=VECTOR('',#10905,1.);
#3428=VECTOR('',#10908,1.);
#3429=VECTOR('',#10909,1.);
#3430=VECTOR('',#10910,1.);
#3431=VECTOR('',#10913,1.);
#3432=VECTOR('',#10914,1.);
#3433=VECTOR('',#10915,1.);
#3434=VECTOR('',#10916,1.);
#3435=VECTOR('',#10919,1.);
#3436=VECTOR('',#10920,1.);
#3437=VECTOR('',#10921,1.);
#3438=VECTOR('',#10924,1.);
#3439=VECTOR('',#10925,1.);
#3440=VECTOR('',#10926,1.);
#3441=VECTOR('',#10929,1.);
#3442=VECTOR('',#10930,1.);
#3443=VECTOR('',#10931,1.);
#3444=VECTOR('',#10934,1.);
#3445=VECTOR('',#10935,1.);
#3446=VECTOR('',#10936,1.);
#3447=VECTOR('',#10939,1.);
#3448=VECTOR('',#10940,1.);
#3449=VECTOR('',#10941,1.);
#3450=VECTOR('',#10944,1.);
#3451=VECTOR('',#10945,1.);
#3452=VECTOR('',#10946,1.);
#3453=VECTOR('',#10949,1.);
#3454=VECTOR('',#10950,1.);
#3455=VECTOR('',#10951,1.);
#3456=VECTOR('',#10954,1.);
#3457=VECTOR('',#10955,1.);
#3458=VECTOR('',#10956,1.);
#3459=VECTOR('',#10961,0.21);
#3460=VECTOR('',#10966,1.);
#3461=VECTOR('',#10967,1.);
#3462=VECTOR('',#10968,1.);
#3463=VECTOR('',#10971,1.);
#3464=VECTOR('',#10972,1.);
#3465=VECTOR('',#10973,1.);
#3466=VECTOR('',#10976,1.);
#3467=VECTOR('',#10977,1.);
#3468=VECTOR('',#10980,1.);
#3469=VECTOR('',#10981,1.);
#3470=VECTOR('',#10982,1.);
#3471=VECTOR('',#10985,1.);
#3472=VECTOR('',#10986,1.);
#3473=VECTOR('',#10989,1.);
#3474=VECTOR('',#10990,1.);
#3475=VECTOR('',#10991,1.);
#3476=VECTOR('',#10994,1.);
#3477=VECTOR('',#10995,1.);
#3478=VECTOR('',#10998,1.);
#3479=VECTOR('',#10999,1.);
#3480=VECTOR('',#11008,1.);
#3481=VECTOR('',#11009,1.);
#3482=VECTOR('',#11010,1.);
#3483=VECTOR('',#11011,1.);
#3484=VECTOR('',#11014,1.);
#3485=VECTOR('',#11015,1.);
#3486=VECTOR('',#11016,1.);
#3487=VECTOR('',#11019,1.);
#3488=VECTOR('',#11020,1.);
#3489=VECTOR('',#11021,1.);
#3490=VECTOR('',#11026,1.);
#3491=VECTOR('',#11027,1.);
#3492=VECTOR('',#11028,1.);
#3493=VECTOR('',#11029,1.);
#3494=VECTOR('',#11030,1.);
#3495=VECTOR('',#11031,1.);
#3496=VECTOR('',#11032,1.);
#3497=VECTOR('',#11035,1.);
#3498=VECTOR('',#11036,1.);
#3499=VECTOR('',#11039,1.);
#3500=VECTOR('',#11040,1.);
#3501=VECTOR('',#11043,1.);
#3502=VECTOR('',#11044,1.);
#3503=VECTOR('',#11045,1.);
#3504=VECTOR('',#11046,1.);
#3505=VECTOR('',#11047,1.);
#3506=VECTOR('',#11050,1.);
#3507=VECTOR('',#11053,1.);
#3508=VECTOR('',#11056,1.);
#3509=VECTOR('',#11061,0.21);
#3510=VECTOR('',#11070,1.);
#3511=VECTOR('',#11073,1.);
#3512=VECTOR('',#11076,1.);
#3513=VECTOR('',#11083,1.);
#3514=VECTOR('',#11084,1.);
#3515=VECTOR('',#11085,1.);
#3516=VECTOR('',#11086,1.);
#3517=VECTOR('',#11089,1.);
#3518=VECTOR('',#11090,1.);
#3519=VECTOR('',#11091,1.);
#3520=VECTOR('',#11094,1.);
#3521=VECTOR('',#11095,1.);
#3522=VECTOR('',#11096,1.);
#3523=VECTOR('',#11099,1.);
#3524=VECTOR('',#11100,1.);
#3525=VECTOR('',#11101,1.);
#3526=VECTOR('',#11104,1.);
#3527=VECTOR('',#11105,1.);
#3528=VECTOR('',#11106,1.);
#3529=VECTOR('',#11109,1.);
#3530=VECTOR('',#11110,1.);
#3531=VECTOR('',#11127,0.4);
#3532=VECTOR('',#11132,0.425);
#3533=VECTOR('',#11137,0.41);
#3534=VECTOR('',#11146,0.26);
#3535=VECTOR('',#11149,0.25);
#3536=VECTOR('',#11154,1.);
#3537=VECTOR('',#11155,1.);
#3538=VECTOR('',#11156,1.);
#3539=VECTOR('',#11157,1.);
#3540=VECTOR('',#11160,1.);
#3541=VECTOR('',#11161,1.);
#3542=VECTOR('',#11162,1.);
#3543=VECTOR('',#11165,1.);
#3544=VECTOR('',#11166,1.);
#3545=VECTOR('',#11167,1.);
#3546=VECTOR('',#11170,1.);
#3547=VECTOR('',#11171,1.);
#3548=VECTOR('',#11172,1.);
#3549=VECTOR('',#11175,1.);
#3550=VECTOR('',#11176,1.);
#3551=VECTOR('',#11177,1.);
#3552=VECTOR('',#11180,1.);
#3553=VECTOR('',#11181,1.);
#3554=VECTOR('',#11198,0.325);
#3555=VECTOR('',#11203,0.35);
#3556=VECTOR('',#11208,0.335);
#3557=VECTOR('',#11217,0.21);
#3558=VECTOR('',#11220,0.2);
#3559=VECTOR('',#11229,0.164999999999999);
#3560=VECTOR('',#11236,0.25);
#3561=VECTOR('',#11243,0.275);
#3562=VECTOR('',#11250,0.275);
#3563=VECTOR('',#11257,0.275);
#3564=VECTOR('',#11264,0.275);
#3565=VECTOR('',#11269,1.);
#3566=VECTOR('',#11270,1.);
#3567=VECTOR('',#11271,1.);
#3568=VECTOR('',#11272,1.);
#3569=VECTOR('',#11275,1.);
#3570=VECTOR('',#11276,1.);
#3571=VECTOR('',#11277,1.);
#3572=VECTOR('',#11280,1.);
#3573=VECTOR('',#11281,1.);
#3574=VECTOR('',#11282,1.);
#3575=VECTOR('',#11285,1.);
#3576=VECTOR('',#11286,1.);
#3577=VECTOR('',#11297,0.225);
#3578=VECTOR('',#11302,1.);
#3579=VECTOR('',#11303,1.);
#3580=VECTOR('',#11304,1.);
#3581=VECTOR('',#11305,1.);
#3582=VECTOR('',#11308,1.);
#3583=VECTOR('',#11309,1.);
#3584=VECTOR('',#11310,1.);
#3585=VECTOR('',#11313,1.);
#3586=VECTOR('',#11314,1.);
#3587=VECTOR('',#11315,1.);
#3588=VECTOR('',#11318,1.);
#3589=VECTOR('',#11319,1.);
#3590=VECTOR('',#11320,1.);
#3591=VECTOR('',#11323,1.);
#3592=VECTOR('',#11324,1.);
#3593=VECTOR('',#11325,1.);
#3594=VECTOR('',#11328,1.);
#3595=VECTOR('',#11329,1.);
#3596=VECTOR('',#11340,0.33);
#3597=VECTOR('',#11347,1.5);
#3598=VECTOR('',#11360,1.);
#3599=VECTOR('',#11365,1.);
#3600=VECTOR('',#11368,0.21);
#3601=VECTOR('',#11373,1.);
#3602=VECTOR('',#11376,1.);
#3603=VECTOR('',#11381,1.);
#3604=VECTOR('',#11384,0.21);
#3605=VECTOR('',#11389,1.);
#3606=VECTOR('',#11392,1.);
#3607=VECTOR('',#11397,1.);
#3608=VECTOR('',#11400,0.21);
#3609=VECTOR('',#11405,1.);
#3610=VECTOR('',#11408,1.);
#3611=VECTOR('',#11413,1.);
#3612=VECTOR('',#11416,0.21);
#3613=VECTOR('',#11421,1.);
#3614=VECTOR('',#11424,1.);
#3615=VECTOR('',#11425,1.);
#3616=VECTOR('',#11426,1.);
#3617=VECTOR('',#11427,1.);
#3618=VECTOR('',#11428,1.);
#3619=VECTOR('',#11429,1.);
#3620=VECTOR('',#11432,1.);
#3621=VECTOR('',#11433,1.);
#3622=VECTOR('',#11434,1.);
#3623=VECTOR('',#11435,1.);
#3624=VECTOR('',#11436,1.);
#3625=VECTOR('',#11437,1.);
#3626=VECTOR('',#11440,1.);
#3627=VECTOR('',#11441,1.);
#3628=VECTOR('',#11442,1.);
#3629=VECTOR('',#11443,1.);
#3630=VECTOR('',#11444,1.);
#3631=VECTOR('',#11445,1.);
#3632=VECTOR('',#11446,1.);
#3633=VECTOR('',#11447,1.);
#3634=VECTOR('',#11448,1.);
#3635=VECTOR('',#11449,1.);
#3636=VECTOR('',#11452,1.);
#3637=VECTOR('',#11453,1.);
#3638=VECTOR('',#11456,1.);
#3639=VECTOR('',#11457,1.);
#3640=VECTOR('',#11460,1.);
#3641=VECTOR('',#11461,1.);
#3642=VECTOR('',#11464,1.);
#3643=VECTOR('',#11465,1.);
#3644=VECTOR('',#11468,1.);
#3645=VECTOR('',#11471,1.);
#3646=VECTOR('',#11472,1.);
#3647=VECTOR('',#11475,1.);
#3648=VECTOR('',#11476,1.);
#3649=VECTOR('',#11479,1.);
#3650=VECTOR('',#11480,1.);
#3651=VECTOR('',#11483,1.);
#3652=VECTOR('',#11484,1.);
#3653=VECTOR('',#11487,1.);
#3654=VECTOR('',#11494,1.);
#3655=VECTOR('',#11495,1.);
#3656=VECTOR('',#11496,1.);
#3657=VECTOR('',#11497,1.);
#3658=VECTOR('',#11500,1.);
#3659=VECTOR('',#11501,1.);
#3660=VECTOR('',#11502,1.);
#3661=VECTOR('',#11505,1.);
#3662=VECTOR('',#11506,1.);
#3663=VECTOR('',#11507,1.);
#3664=VECTOR('',#11510,1.);
#3665=VECTOR('',#11511,1.);
#3666=VECTOR('',#11512,1.);
#3667=VECTOR('',#11515,1.);
#3668=VECTOR('',#11516,1.);
#3669=VECTOR('',#11517,1.);
#3670=VECTOR('',#11520,1.);
#3671=VECTOR('',#11521,1.);
#3672=VECTOR('',#11522,1.);
#3673=VECTOR('',#11525,1.);
#3674=VECTOR('',#11526,1.);
#3675=VECTOR('',#11527,1.);
#3676=VECTOR('',#11530,1.);
#3677=VECTOR('',#11531,1.);
#3678=VECTOR('',#11540,1.);
#3679=VECTOR('',#11541,1.);
#3680=VECTOR('',#11542,1.);
#3681=VECTOR('',#11543,1.);
#3682=VECTOR('',#11546,1.);
#3683=VECTOR('',#11547,1.);
#3684=VECTOR('',#11548,1.);
#3685=VECTOR('',#11551,1.);
#3686=VECTOR('',#11552,1.);
#3687=VECTOR('',#11553,1.);
#3688=VECTOR('',#11556,1.);
#3689=VECTOR('',#11557,1.);
#3690=VECTOR('',#11558,1.);
#3691=VECTOR('',#11561,1.);
#3692=VECTOR('',#11562,1.);
#3693=VECTOR('',#11563,1.);
#3694=VECTOR('',#11566,1.);
#3695=VECTOR('',#11567,1.);
#3696=VECTOR('',#11568,1.);
#3697=VECTOR('',#11571,1.);
#3698=VECTOR('',#11572,1.);
#3699=VECTOR('',#11573,1.);
#3700=VECTOR('',#11576,1.);
#3701=VECTOR('',#11577,1.);
#3702=VECTOR('',#11594,0.275);
#3703=VECTOR('',#11599,0.265);
#3704=VECTOR('',#11608,0.5);
#3705=VECTOR('',#11623,0.4);
#3706=VECTOR('',#11628,0.425);
#3707=VECTOR('',#11633,0.41);
#3708=VECTOR('',#11642,0.26);
#3709=VECTOR('',#11647,0.25);
#3710=VECTOR('',#11652,0.225);
#3711=VECTOR('',#11657,1.);
#3712=VECTOR('',#11658,1.);
#3713=VECTOR('',#11659,1.);
#3714=VECTOR('',#11660,1.);
#3715=VECTOR('',#11663,1.);
#3716=VECTOR('',#11664,1.);
#3717=VECTOR('',#11665,1.);
#3718=VECTOR('',#11668,1.);
#3719=VECTOR('',#11669,1.);
#3720=VECTOR('',#11670,1.);
#3721=VECTOR('',#11673,1.);
#3722=VECTOR('',#11674,1.);
#3723=VECTOR('',#11675,1.);
#3724=VECTOR('',#11678,1.);
#3725=VECTOR('',#11679,1.);
#3726=VECTOR('',#11680,1.);
#3727=VECTOR('',#11683,1.);
#3728=VECTOR('',#11684,1.);
#3729=VECTOR('',#11695,0.225);
#3730=VECTOR('',#11700,0.215);
#3731=VECTOR('',#11709,0.45);
#3732=VECTOR('',#11724,0.325);
#3733=VECTOR('',#11729,0.35);
#3734=VECTOR('',#11734,0.335);
#3735=VECTOR('',#11743,0.21);
#3736=VECTOR('',#11748,0.2);
#3737=VECTOR('',#11753,0.18);
#3738=VECTOR('',#11758,1.);
#3739=VECTOR('',#11759,1.);
#3740=VECTOR('',#11760,1.);
#3741=VECTOR('',#11761,1.);
#3742=VECTOR('',#11764,1.);
#3743=VECTOR('',#11765,1.);
#3744=VECTOR('',#11766,1.);
#3745=VECTOR('',#11769,1.);
#3746=VECTOR('',#11770,1.);
#3747=VECTOR('',#11771,1.);
#3748=VECTOR('',#11774,1.);
#3749=VECTOR('',#11775,1.);
#3750=VECTOR('',#11776,1.);
#3751=VECTOR('',#11779,1.);
#3752=VECTOR('',#11780,1.);
#3753=VECTOR('',#11781,1.);
#3754=VECTOR('',#11784,1.);
#3755=VECTOR('',#11785,1.);
#3756=VECTOR('',#11870,0.32);
#3757=VECTOR('',#11877,0.6);
#3758=VECTOR('',#11894,0.475);
#3759=VECTOR('',#11899,0.5);
#3760=VECTOR('',#11904,0.485);
#3761=VECTOR('',#11913,0.31);
#3762=VECTOR('',#11918,0.3);
#3763=VECTOR('',#11923,0.27);
#3764=VECTOR('',#11928,1.);
#3765=VECTOR('',#11929,1.);
#3766=VECTOR('',#11930,1.);
#3767=VECTOR('',#11931,1.);
#3768=VECTOR('',#11934,1.);
#3769=VECTOR('',#11935,1.);
#3770=VECTOR('',#11936,1.);
#3771=VECTOR('',#11939,1.);
#3772=VECTOR('',#11940,1.);
#3773=VECTOR('',#11941,1.);
#3774=VECTOR('',#11944,1.);
#3775=VECTOR('',#11945,1.);
#3776=VECTOR('',#11946,1.);
#3777=VECTOR('',#11949,1.);
#3778=VECTOR('',#11950,1.);
#3779=VECTOR('',#11951,1.);
#3780=VECTOR('',#11954,1.);
#3781=VECTOR('',#11955,1.);
#3782=CIRCLE('',#8923,0.165);
#3783=CIRCLE('',#8924,0.165);
#3784=CIRCLE('',#8926,0.164999999999999);
#3785=CIRCLE('',#8927,0.164999999999999);
#3786=CIRCLE('',#8929,0.210000000000001);
#3787=CIRCLE('',#8930,0.210000000000001);
#3788=CIRCLE('',#8932,0.21);
#3789=CIRCLE('',#8933,0.21);
#3790=CIRCLE('',#8935,0.21);
#3791=CIRCLE('',#8936,0.21);
#3792=CIRCLE('',#8938,0.210000000000001);
#3793=CIRCLE('',#8939,0.210000000000001);
#3794=CIRCLE('',#8941,0.274999999999999);
#3795=CIRCLE('',#8942,0.274999999999999);
#3796=CIRCLE('',#8944,0.275);
#3797=CIRCLE('',#8945,0.275);
#3798=CIRCLE('',#8947,0.275);
#3799=CIRCLE('',#8948,0.275);
#3800=CIRCLE('',#8950,0.274999999999999);
#3801=CIRCLE('',#8951,0.274999999999999);
#3802=CIRCLE('',#8953,0.164999999999999);
#3803=CIRCLE('',#8954,0.164999999999999);
#3804=CIRCLE('',#8956,0.164999999999999);
#3805=CIRCLE('',#8957,0.164999999999999);
#3806=CIRCLE('',#8959,0.165);
#3807=CIRCLE('',#8960,0.165);
#3808=CIRCLE('',#8962,0.164999999999999);
#3809=CIRCLE('',#8963,0.164999999999999);
#3810=CIRCLE('',#8972,0.475);
#3811=CIRCLE('',#8973,0.475);
#3812=CIRCLE('',#8975,0.275);
#3813=CIRCLE('',#8977,0.475);
#3814=CIRCLE('',#8978,0.475);
#3815=CIRCLE('',#8980,0.275);
#3816=CIRCLE('',#8982,0.275);
#3817=CIRCLE('',#8984,0.275);
#3818=CIRCLE('',#9000,0.475000000000001);
#3819=CIRCLE('',#9001,0.475000000000001);
#3820=CIRCLE('',#9003,0.274999999999999);
#3821=CIRCLE('',#9005,0.475000000000001);
#3822=CIRCLE('',#9006,0.475000000000001);
#3823=CIRCLE('',#9008,0.274999999999999);
#3824=CIRCLE('',#9010,0.274999999999999);
#3825=CIRCLE('',#9012,0.274999999999999);
#3826=CIRCLE('',#9144,0.225000000000001);
#3827=CIRCLE('',#9145,0.225);
#3828=CIRCLE('',#9147,0.225);
#3829=CIRCLE('',#9149,0.225000000000001);
#3830=CIRCLE('',#9185,0.375);
#3831=CIRCLE('',#9186,0.375);
#3832=CIRCLE('',#9188,0.225);
#3833=CIRCLE('',#9190,0.375);
#3834=CIRCLE('',#9191,0.375);
#3835=CIRCLE('',#9193,0.225);
#3836=CIRCLE('',#9195,0.375);
#3837=CIRCLE('',#9196,0.375);
#3838=CIRCLE('',#9198,0.225);
#3839=CIRCLE('',#9200,0.375);
#3840=CIRCLE('',#9201,0.375);
#3841=CIRCLE('',#9203,0.225000000000001);
#3842=CIRCLE('',#9205,0.225);
#3843=CIRCLE('',#9207,0.225);
#3844=CIRCLE('',#9209,0.225);
#3845=CIRCLE('',#9211,0.225000000000001);
#3846=CIRCLE('',#9264,0.21);
#3847=CIRCLE('',#9265,0.21);
#3848=CIRCLE('',#9280,0.2117);
#3849=CIRCLE('',#9289,0.2117);
#3850=CIRCLE('',#9290,0.2117);
#3851=CIRCLE('',#9292,0.2117);
#3852=CIRCLE('',#9307,0.24505);
#3853=CIRCLE('',#9309,0.375);
#3854=CIRCLE('',#9311,0.425);
#3855=CIRCLE('',#9313,0.425);
#3856=CIRCLE('',#9315,0.395);
#3857=CIRCLE('',#9317,0.27);
#3858=CIRCLE('',#9319,0.24505);
#3859=CIRCLE('',#9331,0.1954);
#3860=CIRCLE('',#9333,0.3);
#3861=CIRCLE('',#9335,0.35);
#3862=CIRCLE('',#9337,0.35);
#3863=CIRCLE('',#9339,0.32);
#3864=CIRCLE('',#9341,0.22);
#3865=CIRCLE('',#9343,0.1954);
#3866=CIRCLE('',#9348,0.164999999999999);
#3867=CIRCLE('',#9349,0.164999999999999);
#3868=CIRCLE('',#9351,0.25);
#3869=CIRCLE('',#9352,0.25);
#3870=CIRCLE('',#9354,0.275);
#3871=CIRCLE('',#9355,0.275);
#3872=CIRCLE('',#9357,0.275);
#3873=CIRCLE('',#9358,0.275);
#3874=CIRCLE('',#9360,0.275);
#3875=CIRCLE('',#9361,0.275);
#3876=CIRCLE('',#9363,0.275);
#3877=CIRCLE('',#9364,0.275);
#3878=CIRCLE('',#9373,0.225);
#3879=CIRCLE('',#9374,0.225);
#3880=CIRCLE('',#9385,0.33);
#3881=CIRCLE('',#9386,0.33);
#3882=CIRCLE('',#9388,1.5);
#3883=CIRCLE('',#9389,1.5);
#3884=CIRCLE('',#9395,0.21);
#3885=CIRCLE('',#9397,0.21);
#3886=CIRCLE('',#9398,0.21);
#3887=CIRCLE('',#9399,0.21);
#3888=CIRCLE('',#9401,0.21);
#3889=CIRCLE('',#9403,0.21);
#3890=CIRCLE('',#9404,0.21);
#3891=CIRCLE('',#9405,0.21);
#3892=CIRCLE('',#9407,0.21);
#3893=CIRCLE('',#9409,0.21);
#3894=CIRCLE('',#9410,0.21);
#3895=CIRCLE('',#9411,0.21);
#3896=CIRCLE('',#9413,0.21);
#3897=CIRCLE('',#9415,0.21);
#3898=CIRCLE('',#9416,0.21);
#3899=CIRCLE('',#9417,0.21);
#3900=CIRCLE('',#9459,0.285);
#3901=CIRCLE('',#9460,0.265);
#3902=CIRCLE('',#9462,0.265);
#3903=CIRCLE('',#9464,0.5);
#3904=CIRCLE('',#9466,0.5);
#3905=CIRCLE('',#9470,0.375);
#3906=CIRCLE('',#9472,0.425);
#3907=CIRCLE('',#9474,0.425);
#3908=CIRCLE('',#9476,0.395);
#3909=CIRCLE('',#9478,0.27);
#3910=CIRCLE('',#9480,0.24505);
#3911=CIRCLE('',#9482,0.24505);
#3912=CIRCLE('',#9484,0.2);
#3913=CIRCLE('',#9496,0.235);
#3914=CIRCLE('',#9497,0.215);
#3915=CIRCLE('',#9499,0.215);
#3916=CIRCLE('',#9501,0.45);
#3917=CIRCLE('',#9503,0.45);
#3918=CIRCLE('',#9507,0.3);
#3919=CIRCLE('',#9509,0.35);
#3920=CIRCLE('',#9511,0.35);
#3921=CIRCLE('',#9513,0.32);
#3922=CIRCLE('',#9515,0.22);
#3923=CIRCLE('',#9517,0.1954);
#3924=CIRCLE('',#9519,0.1954);
#3925=CIRCLE('',#9521,0.16);
#3926=CIRCLE('',#9570,0.32);
#3927=CIRCLE('',#9571,0.32);
#3928=CIRCLE('',#9573,0.6);
#3929=CIRCLE('',#9574,0.6);
#3930=CIRCLE('',#9579,0.45);
#3931=CIRCLE('',#9581,0.5);
#3932=CIRCLE('',#9583,0.5);
#3933=CIRCLE('',#9585,0.47);
#3934=CIRCLE('',#9587,0.32);
#3935=CIRCLE('',#9589,0.2942);
#3936=CIRCLE('',#9591,0.2942);
#3937=CIRCLE('',#9593,0.24);
#3938=VERTEX_POINT('',#12000);
#3939=VERTEX_POINT('',#12002);
#3940=VERTEX_POINT('',#12006);
#3941=VERTEX_POINT('',#12008);
#3942=VERTEX_POINT('',#12012);
#3943=VERTEX_POINT('',#12014);
#3944=VERTEX_POINT('',#12018);
#3945=VERTEX_POINT('',#12020);
#3946=VERTEX_POINT('',#12024);
#3947=VERTEX_POINT('',#12026);
#3948=VERTEX_POINT('',#12030);
#3949=VERTEX_POINT('',#12032);
#3950=VERTEX_POINT('',#12036);
#3951=VERTEX_POINT('',#12038);
#3952=VERTEX_POINT('',#12042);
#3953=VERTEX_POINT('',#12044);
#3954=VERTEX_POINT('',#12048);
#3955=VERTEX_POINT('',#12050);
#3956=VERTEX_POINT('',#12054);
#3957=VERTEX_POINT('',#12056);
#3958=VERTEX_POINT('',#12060);
#3959=VERTEX_POINT('',#12062);
#3960=VERTEX_POINT('',#12066);
#3961=VERTEX_POINT('',#12068);
#3962=VERTEX_POINT('',#12072);
#3963=VERTEX_POINT('',#12074);
#3964=VERTEX_POINT('',#12078);
#3965=VERTEX_POINT('',#12080);
#3966=VERTEX_POINT('',#12084);
#3967=VERTEX_POINT('',#12085);
#3968=VERTEX_POINT('',#12087);
#3969=VERTEX_POINT('',#12089);
#3970=VERTEX_POINT('',#12093);
#3971=VERTEX_POINT('',#12095);
#3972=VERTEX_POINT('',#12099);
#3973=VERTEX_POINT('',#12101);
#3974=VERTEX_POINT('',#12111);
#3975=VERTEX_POINT('',#12113);
#3976=VERTEX_POINT('',#12117);
#3977=VERTEX_POINT('',#12120);
#3978=VERTEX_POINT('',#12122);
#3979=VERTEX_POINT('',#12126);
#3980=VERTEX_POINT('',#12129);
#3981=VERTEX_POINT('',#12133);
#3982=VERTEX_POINT('',#12137);
#3983=VERTEX_POINT('',#12138);
#3984=VERTEX_POINT('',#12140);
#3985=VERTEX_POINT('',#12142);
#3986=VERTEX_POINT('',#12146);
#3987=VERTEX_POINT('',#12148);
#3988=VERTEX_POINT('',#12152);
#3989=VERTEX_POINT('',#12154);
#3990=VERTEX_POINT('',#12164);
#3991=VERTEX_POINT('',#12165);
#3992=VERTEX_POINT('',#12167);
#3993=VERTEX_POINT('',#12169);
#3994=VERTEX_POINT('',#12173);
#3995=VERTEX_POINT('',#12175);
#3996=VERTEX_POINT('',#12179);
#3997=VERTEX_POINT('',#12181);
#3998=VERTEX_POINT('',#12191);
#3999=VERTEX_POINT('',#12193);
#4000=VERTEX_POINT('',#12197);
#4001=VERTEX_POINT('',#12200);
#4002=VERTEX_POINT('',#12202);
#4003=VERTEX_POINT('',#12206);
#4004=VERTEX_POINT('',#12209);
#4005=VERTEX_POINT('',#12213);
#4006=VERTEX_POINT('',#12217);
#4007=VERTEX_POINT('',#12218);
#4008=VERTEX_POINT('',#12220);
#4009=VERTEX_POINT('',#12222);
#4010=VERTEX_POINT('',#12226);
#4011=VERTEX_POINT('',#12228);
#4012=VERTEX_POINT('',#12232);
#4013=VERTEX_POINT('',#12234);
#4014=VERTEX_POINT('',#12244);
#4015=VERTEX_POINT('',#12245);
#4016=VERTEX_POINT('',#12247);
#4017=VERTEX_POINT('',#12249);
#4018=VERTEX_POINT('',#12253);
#4019=VERTEX_POINT('',#12255);
#4020=VERTEX_POINT('',#12259);
#4021=VERTEX_POINT('',#12261);
#4022=VERTEX_POINT('',#12271);
#4023=VERTEX_POINT('',#12272);
#4024=VERTEX_POINT('',#12274);
#4025=VERTEX_POINT('',#12276);
#4026=VERTEX_POINT('',#12280);
#4027=VERTEX_POINT('',#12282);
#4028=VERTEX_POINT('',#12286);
#4029=VERTEX_POINT('',#12288);
#4030=VERTEX_POINT('',#12294);
#4031=VERTEX_POINT('',#12295);
#4032=VERTEX_POINT('',#12297);
#4033=VERTEX_POINT('',#12299);
#4034=VERTEX_POINT('',#12303);
#4035=VERTEX_POINT('',#12305);
#4036=VERTEX_POINT('',#12309);
#4037=VERTEX_POINT('',#12311);
#4038=VERTEX_POINT('',#12317);
#4039=VERTEX_POINT('',#12318);
#4040=VERTEX_POINT('',#12320);
#4041=VERTEX_POINT('',#12322);
#4042=VERTEX_POINT('',#12326);
#4043=VERTEX_POINT('',#12328);
#4044=VERTEX_POINT('',#12332);
#4045=VERTEX_POINT('',#12334);
#4046=VERTEX_POINT('',#12340);
#4047=VERTEX_POINT('',#12341);
#4048=VERTEX_POINT('',#12343);
#4049=VERTEX_POINT('',#12345);
#4050=VERTEX_POINT('',#12349);
#4051=VERTEX_POINT('',#12351);
#4052=VERTEX_POINT('',#12355);
#4053=VERTEX_POINT('',#12357);
#4054=VERTEX_POINT('',#12363);
#4055=VERTEX_POINT('',#12364);
#4056=VERTEX_POINT('',#12366);
#4057=VERTEX_POINT('',#12368);
#4058=VERTEX_POINT('',#12372);
#4059=VERTEX_POINT('',#12374);
#4060=VERTEX_POINT('',#12378);
#4061=VERTEX_POINT('',#12380);
#4062=VERTEX_POINT('',#12386);
#4063=VERTEX_POINT('',#12387);
#4064=VERTEX_POINT('',#12389);
#4065=VERTEX_POINT('',#12391);
#4066=VERTEX_POINT('',#12395);
#4067=VERTEX_POINT('',#12397);
#4068=VERTEX_POINT('',#12401);
#4069=VERTEX_POINT('',#12403);
#4070=VERTEX_POINT('',#12409);
#4071=VERTEX_POINT('',#12410);
#4072=VERTEX_POINT('',#12412);
#4073=VERTEX_POINT('',#12414);
#4074=VERTEX_POINT('',#12418);
#4075=VERTEX_POINT('',#12420);
#4076=VERTEX_POINT('',#12424);
#4077=VERTEX_POINT('',#12426);
#4078=VERTEX_POINT('',#12432);
#4079=VERTEX_POINT('',#12433);
#4080=VERTEX_POINT('',#12435);
#4081=VERTEX_POINT('',#12437);
#4082=VERTEX_POINT('',#12441);
#4083=VERTEX_POINT('',#12443);
#4084=VERTEX_POINT('',#12447);
#4085=VERTEX_POINT('',#12449);
#4086=VERTEX_POINT('',#12455);
#4087=VERTEX_POINT('',#12456);
#4088=VERTEX_POINT('',#12458);
#4089=VERTEX_POINT('',#12460);
#4090=VERTEX_POINT('',#12464);
#4091=VERTEX_POINT('',#12466);
#4092=VERTEX_POINT('',#12470);
#4093=VERTEX_POINT('',#12472);
#4094=VERTEX_POINT('',#12478);
#4095=VERTEX_POINT('',#12479);
#4096=VERTEX_POINT('',#12481);
#4097=VERTEX_POINT('',#12483);
#4098=VERTEX_POINT('',#12487);
#4099=VERTEX_POINT('',#12489);
#4100=VERTEX_POINT('',#12493);
#4101=VERTEX_POINT('',#12495);
#4102=VERTEX_POINT('',#12501);
#4103=VERTEX_POINT('',#12502);
#4104=VERTEX_POINT('',#12504);
#4105=VERTEX_POINT('',#12506);
#4106=VERTEX_POINT('',#12510);
#4107=VERTEX_POINT('',#12512);
#4108=VERTEX_POINT('',#12516);
#4109=VERTEX_POINT('',#12518);
#4110=VERTEX_POINT('',#12524);
#4111=VERTEX_POINT('',#12525);
#4112=VERTEX_POINT('',#12527);
#4113=VERTEX_POINT('',#12529);
#4114=VERTEX_POINT('',#12533);
#4115=VERTEX_POINT('',#12535);
#4116=VERTEX_POINT('',#12539);
#4117=VERTEX_POINT('',#12541);
#4118=VERTEX_POINT('',#12547);
#4119=VERTEX_POINT('',#12548);
#4120=VERTEX_POINT('',#12550);
#4121=VERTEX_POINT('',#12552);
#4122=VERTEX_POINT('',#12556);
#4123=VERTEX_POINT('',#12558);
#4124=VERTEX_POINT('',#12562);
#4125=VERTEX_POINT('',#12564);
#4126=VERTEX_POINT('',#12570);
#4127=VERTEX_POINT('',#12571);
#4128=VERTEX_POINT('',#12573);
#4129=VERTEX_POINT('',#12575);
#4130=VERTEX_POINT('',#12579);
#4131=VERTEX_POINT('',#12581);
#4132=VERTEX_POINT('',#12585);
#4133=VERTEX_POINT('',#12587);
#4134=VERTEX_POINT('',#12593);
#4135=VERTEX_POINT('',#12594);
#4136=VERTEX_POINT('',#12596);
#4137=VERTEX_POINT('',#12598);
#4138=VERTEX_POINT('',#12602);
#4139=VERTEX_POINT('',#12604);
#4140=VERTEX_POINT('',#12608);
#4141=VERTEX_POINT('',#12610);
#4142=VERTEX_POINT('',#12616);
#4143=VERTEX_POINT('',#12617);
#4144=VERTEX_POINT('',#12619);
#4145=VERTEX_POINT('',#12621);
#4146=VERTEX_POINT('',#12625);
#4147=VERTEX_POINT('',#12627);
#4148=VERTEX_POINT('',#12631);
#4149=VERTEX_POINT('',#12633);
#4150=VERTEX_POINT('',#12639);
#4151=VERTEX_POINT('',#12640);
#4152=VERTEX_POINT('',#12642);
#4153=VERTEX_POINT('',#12644);
#4154=VERTEX_POINT('',#12648);
#4155=VERTEX_POINT('',#12650);
#4156=VERTEX_POINT('',#12654);
#4157=VERTEX_POINT('',#12656);
#4158=VERTEX_POINT('',#12662);
#4159=VERTEX_POINT('',#12663);
#4160=VERTEX_POINT('',#12665);
#4161=VERTEX_POINT('',#12667);
#4162=VERTEX_POINT('',#12671);
#4163=VERTEX_POINT('',#12673);
#4164=VERTEX_POINT('',#12677);
#4165=VERTEX_POINT('',#12679);
#4166=VERTEX_POINT('',#12685);
#4167=VERTEX_POINT('',#12686);
#4168=VERTEX_POINT('',#12688);
#4169=VERTEX_POINT('',#12690);
#4170=VERTEX_POINT('',#12694);
#4171=VERTEX_POINT('',#12696);
#4172=VERTEX_POINT('',#12700);
#4173=VERTEX_POINT('',#12702);
#4174=VERTEX_POINT('',#12708);
#4175=VERTEX_POINT('',#12709);
#4176=VERTEX_POINT('',#12711);
#4177=VERTEX_POINT('',#12713);
#4178=VERTEX_POINT('',#12717);
#4179=VERTEX_POINT('',#12719);
#4180=VERTEX_POINT('',#12723);
#4181=VERTEX_POINT('',#12725);
#4182=VERTEX_POINT('',#12731);
#4183=VERTEX_POINT('',#12732);
#4184=VERTEX_POINT('',#12734);
#4185=VERTEX_POINT('',#12736);
#4186=VERTEX_POINT('',#12740);
#4187=VERTEX_POINT('',#12742);
#4188=VERTEX_POINT('',#12746);
#4189=VERTEX_POINT('',#12748);
#4190=VERTEX_POINT('',#12754);
#4191=VERTEX_POINT('',#12755);
#4192=VERTEX_POINT('',#12757);
#4193=VERTEX_POINT('',#12759);
#4194=VERTEX_POINT('',#12763);
#4195=VERTEX_POINT('',#12765);
#4196=VERTEX_POINT('',#12769);
#4197=VERTEX_POINT('',#12771);
#4198=VERTEX_POINT('',#12777);
#4199=VERTEX_POINT('',#12778);
#4200=VERTEX_POINT('',#12780);
#4201=VERTEX_POINT('',#12782);
#4202=VERTEX_POINT('',#12786);
#4203=VERTEX_POINT('',#12788);
#4204=VERTEX_POINT('',#12792);
#4205=VERTEX_POINT('',#12794);
#4206=VERTEX_POINT('',#12800);
#4207=VERTEX_POINT('',#12801);
#4208=VERTEX_POINT('',#12803);
#4209=VERTEX_POINT('',#12805);
#4210=VERTEX_POINT('',#12809);
#4211=VERTEX_POINT('',#12811);
#4212=VERTEX_POINT('',#12815);
#4213=VERTEX_POINT('',#12817);
#4214=VERTEX_POINT('',#12823);
#4215=VERTEX_POINT('',#12824);
#4216=VERTEX_POINT('',#12826);
#4217=VERTEX_POINT('',#12828);
#4218=VERTEX_POINT('',#12832);
#4219=VERTEX_POINT('',#12834);
#4220=VERTEX_POINT('',#12838);
#4221=VERTEX_POINT('',#12840);
#4222=VERTEX_POINT('',#12846);
#4223=VERTEX_POINT('',#12847);
#4224=VERTEX_POINT('',#12849);
#4225=VERTEX_POINT('',#12851);
#4226=VERTEX_POINT('',#12855);
#4227=VERTEX_POINT('',#12857);
#4228=VERTEX_POINT('',#12861);
#4229=VERTEX_POINT('',#12863);
#4230=VERTEX_POINT('',#12869);
#4231=VERTEX_POINT('',#12870);
#4232=VERTEX_POINT('',#12872);
#4233=VERTEX_POINT('',#12874);
#4234=VERTEX_POINT('',#12878);
#4235=VERTEX_POINT('',#12880);
#4236=VERTEX_POINT('',#12884);
#4237=VERTEX_POINT('',#12886);
#4238=VERTEX_POINT('',#12892);
#4239=VERTEX_POINT('',#12893);
#4240=VERTEX_POINT('',#12895);
#4241=VERTEX_POINT('',#12897);
#4242=VERTEX_POINT('',#12901);
#4243=VERTEX_POINT('',#12903);
#4244=VERTEX_POINT('',#12907);
#4245=VERTEX_POINT('',#12909);
#4246=VERTEX_POINT('',#12915);
#4247=VERTEX_POINT('',#12916);
#4248=VERTEX_POINT('',#12918);
#4249=VERTEX_POINT('',#12920);
#4250=VERTEX_POINT('',#12924);
#4251=VERTEX_POINT('',#12926);
#4252=VERTEX_POINT('',#12930);
#4253=VERTEX_POINT('',#12932);
#4254=VERTEX_POINT('',#12939);
#4255=VERTEX_POINT('',#12941);
#4256=VERTEX_POINT('',#12943);
#4257=VERTEX_POINT('',#12945);
#4258=VERTEX_POINT('',#12975);
#4259=VERTEX_POINT('',#12977);
#4260=VERTEX_POINT('',#12980);
#4261=VERTEX_POINT('',#12984);
#4262=VERTEX_POINT('',#12988);
#4263=VERTEX_POINT('',#12989);
#4264=VERTEX_POINT('',#12994);
#4265=VERTEX_POINT('',#12998);
#4266=VERTEX_POINT('',#13006);
#4267=VERTEX_POINT('',#13007);
#4268=VERTEX_POINT('',#13009);
#4269=VERTEX_POINT('',#13011);
#4270=VERTEX_POINT('',#13015);
#4271=VERTEX_POINT('',#13017);
#4272=VERTEX_POINT('',#13021);
#4273=VERTEX_POINT('',#13023);
#4274=VERTEX_POINT('',#13033);
#4275=VERTEX_POINT('',#13034);
#4276=VERTEX_POINT('',#13036);
#4277=VERTEX_POINT('',#13038);
#4278=VERTEX_POINT('',#13042);
#4279=VERTEX_POINT('',#13044);
#4280=VERTEX_POINT('',#13048);
#4281=VERTEX_POINT('',#13050);
#4282=VERTEX_POINT('',#13060);
#4283=VERTEX_POINT('',#13061);
#4284=VERTEX_POINT('',#13063);
#4285=VERTEX_POINT('',#13065);
#4286=VERTEX_POINT('',#13069);
#4287=VERTEX_POINT('',#13071);
#4288=VERTEX_POINT('',#13075);
#4289=VERTEX_POINT('',#13077);
#4290=VERTEX_POINT('',#13087);
#4291=VERTEX_POINT('',#13088);
#4292=VERTEX_POINT('',#13090);
#4293=VERTEX_POINT('',#13092);
#4294=VERTEX_POINT('',#13096);
#4295=VERTEX_POINT('',#13098);
#4296=VERTEX_POINT('',#13102);
#4297=VERTEX_POINT('',#13104);
#4298=VERTEX_POINT('',#13114);
#4299=VERTEX_POINT('',#13116);
#4300=VERTEX_POINT('',#13120);
#4301=VERTEX_POINT('',#13123);
#4302=VERTEX_POINT('',#13125);
#4303=VERTEX_POINT('',#13129);
#4304=VERTEX_POINT('',#13132);
#4305=VERTEX_POINT('',#13134);
#4306=VERTEX_POINT('',#13138);
#4307=VERTEX_POINT('',#13141);
#4308=VERTEX_POINT('',#13143);
#4309=VERTEX_POINT('',#13147);
#4310=VERTEX_POINT('',#13150);
#4311=VERTEX_POINT('',#13154);
#4312=VERTEX_POINT('',#13158);
#4313=VERTEX_POINT('',#13162);
#4314=VERTEX_POINT('',#13166);
#4315=VERTEX_POINT('',#13167);
#4316=VERTEX_POINT('',#13169);
#4317=VERTEX_POINT('',#13171);
#4318=VERTEX_POINT('',#13175);
#4319=VERTEX_POINT('',#13177);
#4320=VERTEX_POINT('',#13181);
#4321=VERTEX_POINT('',#13183);
#4322=VERTEX_POINT('',#13187);
#4323=VERTEX_POINT('',#13189);
#4324=VERTEX_POINT('',#13193);
#4325=VERTEX_POINT('',#13195);
#4326=VERTEX_POINT('',#13199);
#4327=VERTEX_POINT('',#13201);
#4328=VERTEX_POINT('',#13205);
#4329=VERTEX_POINT('',#13207);
#4330=VERTEX_POINT('',#13211);
#4331=VERTEX_POINT('',#13213);
#4332=VERTEX_POINT('',#13217);
#4333=VERTEX_POINT('',#13219);
#4334=VERTEX_POINT('',#13223);
#4335=VERTEX_POINT('',#13225);
#4336=VERTEX_POINT('',#13229);
#4337=VERTEX_POINT('',#13231);
#4338=VERTEX_POINT('',#13241);
#4339=VERTEX_POINT('',#13242);
#4340=VERTEX_POINT('',#13244);
#4341=VERTEX_POINT('',#13246);
#4342=VERTEX_POINT('',#13250);
#4343=VERTEX_POINT('',#13252);
#4344=VERTEX_POINT('',#13256);
#4345=VERTEX_POINT('',#13258);
#4346=VERTEX_POINT('',#13262);
#4347=VERTEX_POINT('',#13264);
#4348=VERTEX_POINT('',#13268);
#4349=VERTEX_POINT('',#13270);
#4350=VERTEX_POINT('',#13274);
#4351=VERTEX_POINT('',#13276);
#4352=VERTEX_POINT('',#13280);
#4353=VERTEX_POINT('',#13282);
#4354=VERTEX_POINT('',#13286);
#4355=VERTEX_POINT('',#13288);
#4356=VERTEX_POINT('',#13292);
#4357=VERTEX_POINT('',#13294);
#4358=VERTEX_POINT('',#13298);
#4359=VERTEX_POINT('',#13299);
#4360=VERTEX_POINT('',#13301);
#4361=VERTEX_POINT('',#13303);
#4362=VERTEX_POINT('',#13307);
#4363=VERTEX_POINT('',#13309);
#4364=VERTEX_POINT('',#13313);
#4365=VERTEX_POINT('',#13315);
#4366=VERTEX_POINT('',#13319);
#4367=VERTEX_POINT('',#13321);
#4368=VERTEX_POINT('',#13325);
#4369=VERTEX_POINT('',#13327);
#4370=VERTEX_POINT('',#13331);
#4371=VERTEX_POINT('',#13333);
#4372=VERTEX_POINT('',#13337);
#4373=VERTEX_POINT('',#13339);
#4374=VERTEX_POINT('',#13343);
#4375=VERTEX_POINT('',#13345);
#4376=VERTEX_POINT('',#13349);
#4377=VERTEX_POINT('',#13351);
#4378=VERTEX_POINT('',#13355);
#4379=VERTEX_POINT('',#13356);
#4380=VERTEX_POINT('',#13358);
#4381=VERTEX_POINT('',#13360);
#4382=VERTEX_POINT('',#13364);
#4383=VERTEX_POINT('',#13366);
#4384=VERTEX_POINT('',#13370);
#4385=VERTEX_POINT('',#13372);
#4386=VERTEX_POINT('',#13376);
#4387=VERTEX_POINT('',#13378);
#4388=VERTEX_POINT('',#13382);
#4389=VERTEX_POINT('',#13384);
#4390=VERTEX_POINT('',#13388);
#4391=VERTEX_POINT('',#13390);
#4392=VERTEX_POINT('',#13394);
#4393=VERTEX_POINT('',#13396);
#4394=VERTEX_POINT('',#13400);
#4395=VERTEX_POINT('',#13402);
#4396=VERTEX_POINT('',#13406);
#4397=VERTEX_POINT('',#13408);
#4398=VERTEX_POINT('',#13412);
#4399=VERTEX_POINT('',#13413);
#4400=VERTEX_POINT('',#13415);
#4401=VERTEX_POINT('',#13417);
#4402=VERTEX_POINT('',#13421);
#4403=VERTEX_POINT('',#13423);
#4404=VERTEX_POINT('',#13427);
#4405=VERTEX_POINT('',#13429);
#4406=VERTEX_POINT('',#13433);
#4407=VERTEX_POINT('',#13435);
#4408=VERTEX_POINT('',#13439);
#4409=VERTEX_POINT('',#13441);
#4410=VERTEX_POINT('',#13445);
#4411=VERTEX_POINT('',#13447);
#4412=VERTEX_POINT('',#13451);
#4413=VERTEX_POINT('',#13453);
#4414=VERTEX_POINT('',#13457);
#4415=VERTEX_POINT('',#13459);
#4416=VERTEX_POINT('',#13463);
#4417=VERTEX_POINT('',#13465);
#4418=VERTEX_POINT('',#13469);
#4419=VERTEX_POINT('',#13471);
#4420=VERTEX_POINT('',#13475);
#4421=VERTEX_POINT('',#13477);
#4422=VERTEX_POINT('',#13481);
#4423=VERTEX_POINT('',#13483);
#4424=VERTEX_POINT('',#13490);
#4425=VERTEX_POINT('',#13492);
#4426=VERTEX_POINT('',#13499);
#4427=VERTEX_POINT('',#13501);
#4428=VERTEX_POINT('',#13514);
#4429=VERTEX_POINT('',#13515);
#4430=VERTEX_POINT('',#13517);
#4431=VERTEX_POINT('',#13519);
#4432=VERTEX_POINT('',#13523);
#4433=VERTEX_POINT('',#13525);
#4434=VERTEX_POINT('',#13529);
#4435=VERTEX_POINT('',#13531);
#4436=VERTEX_POINT('',#13534);
#4437=VERTEX_POINT('',#13537);
#4438=VERTEX_POINT('',#13539);
#4439=VERTEX_POINT('',#13541);
#4440=VERTEX_POINT('',#13543);
#4441=VERTEX_POINT('',#13545);
#4442=VERTEX_POINT('',#13547);
#4443=VERTEX_POINT('',#13551);
#4444=VERTEX_POINT('',#13555);
#4445=VERTEX_POINT('',#13559);
#4446=VERTEX_POINT('',#13561);
#4447=VERTEX_POINT('',#13563);
#4448=VERTEX_POINT('',#13565);
#4449=VERTEX_POINT('',#13571);
#4450=VERTEX_POINT('',#13573);
#4451=VERTEX_POINT('',#13577);
#4452=VERTEX_POINT('',#13580);
#4453=VERTEX_POINT('',#13582);
#4454=VERTEX_POINT('',#13594);
#4455=VERTEX_POINT('',#13595);
#4456=VERTEX_POINT('',#13597);
#4457=VERTEX_POINT('',#13599);
#4458=VERTEX_POINT('',#13603);
#4459=VERTEX_POINT('',#13605);
#4460=VERTEX_POINT('',#13609);
#4461=VERTEX_POINT('',#13611);
#4462=VERTEX_POINT('',#13615);
#4463=VERTEX_POINT('',#13617);
#4464=VERTEX_POINT('',#13621);
#4465=VERTEX_POINT('',#13623);
#4466=VERTEX_POINT('',#13632);
#4467=VERTEX_POINT('',#13635);
#4468=VERTEX_POINT('',#13638);
#4469=VERTEX_POINT('',#13642);
#4470=VERTEX_POINT('',#13646);
#4471=VERTEX_POINT('',#13650);
#4472=VERTEX_POINT('',#13653);
#4473=VERTEX_POINT('',#13660);
#4474=VERTEX_POINT('',#13661);
#4475=VERTEX_POINT('',#13663);
#4476=VERTEX_POINT('',#13665);
#4477=VERTEX_POINT('',#13669);
#4478=VERTEX_POINT('',#13671);
#4479=VERTEX_POINT('',#13675);
#4480=VERTEX_POINT('',#13677);
#4481=VERTEX_POINT('',#13681);
#4482=VERTEX_POINT('',#13683);
#4483=VERTEX_POINT('',#13687);
#4484=VERTEX_POINT('',#13689);
#4485=VERTEX_POINT('',#13698);
#4486=VERTEX_POINT('',#13701);
#4487=VERTEX_POINT('',#13704);
#4488=VERTEX_POINT('',#13708);
#4489=VERTEX_POINT('',#13712);
#4490=VERTEX_POINT('',#13716);
#4491=VERTEX_POINT('',#13719);
#4492=VERTEX_POINT('',#13727);
#4493=VERTEX_POINT('',#13729);
#4494=VERTEX_POINT('',#13733);
#4495=VERTEX_POINT('',#13735);
#4496=VERTEX_POINT('',#13739);
#4497=VERTEX_POINT('',#13741);
#4498=VERTEX_POINT('',#13745);
#4499=VERTEX_POINT('',#13747);
#4500=VERTEX_POINT('',#13751);
#4501=VERTEX_POINT('',#13753);
#4502=VERTEX_POINT('',#13757);
#4503=VERTEX_POINT('',#13759);
#4504=VERTEX_POINT('',#13763);
#4505=VERTEX_POINT('',#13764);
#4506=VERTEX_POINT('',#13766);
#4507=VERTEX_POINT('',#13768);
#4508=VERTEX_POINT('',#13772);
#4509=VERTEX_POINT('',#13774);
#4510=VERTEX_POINT('',#13778);
#4511=VERTEX_POINT('',#13780);
#4512=VERTEX_POINT('',#13790);
#4513=VERTEX_POINT('',#13792);
#4514=VERTEX_POINT('',#13796);
#4515=VERTEX_POINT('',#13797);
#4516=VERTEX_POINT('',#13799);
#4517=VERTEX_POINT('',#13801);
#4518=VERTEX_POINT('',#13805);
#4519=VERTEX_POINT('',#13807);
#4520=VERTEX_POINT('',#13811);
#4521=VERTEX_POINT('',#13813);
#4522=VERTEX_POINT('',#13817);
#4523=VERTEX_POINT('',#13819);
#4524=VERTEX_POINT('',#13823);
#4525=VERTEX_POINT('',#13825);
#4526=VERTEX_POINT('',#13835);
#4527=VERTEX_POINT('',#13837);
#4528=VERTEX_POINT('',#13841);
#4529=VERTEX_POINT('',#13843);
#4530=VERTEX_POINT('',#13851);
#4531=VERTEX_POINT('',#13852);
#4532=VERTEX_POINT('',#13856);
#4533=VERTEX_POINT('',#13858);
#4534=VERTEX_POINT('',#13860);
#4535=VERTEX_POINT('',#13863);
#4536=VERTEX_POINT('',#13867);
#4537=VERTEX_POINT('',#13868);
#4538=VERTEX_POINT('',#13872);
#4539=VERTEX_POINT('',#13874);
#4540=VERTEX_POINT('',#13876);
#4541=VERTEX_POINT('',#13879);
#4542=VERTEX_POINT('',#13883);
#4543=VERTEX_POINT('',#13884);
#4544=VERTEX_POINT('',#13888);
#4545=VERTEX_POINT('',#13890);
#4546=VERTEX_POINT('',#13892);
#4547=VERTEX_POINT('',#13895);
#4548=VERTEX_POINT('',#13899);
#4549=VERTEX_POINT('',#13900);
#4550=VERTEX_POINT('',#13904);
#4551=VERTEX_POINT('',#13906);
#4552=VERTEX_POINT('',#13908);
#4553=VERTEX_POINT('',#13911);
#4554=VERTEX_POINT('',#13916);
#4555=VERTEX_POINT('',#13918);
#4556=VERTEX_POINT('',#13920);
#4557=VERTEX_POINT('',#13922);
#4558=VERTEX_POINT('',#13927);
#4559=VERTEX_POINT('',#13929);
#4560=VERTEX_POINT('',#13931);
#4561=VERTEX_POINT('',#13933);
#4562=VERTEX_POINT('',#13937);
#4563=VERTEX_POINT('',#13939);
#4564=VERTEX_POINT('',#13941);
#4565=VERTEX_POINT('',#13943);
#4566=VERTEX_POINT('',#13946);
#4567=VERTEX_POINT('',#13948);
#4568=VERTEX_POINT('',#13950);
#4569=VERTEX_POINT('',#13952);
#4570=VERTEX_POINT('',#13956);
#4571=VERTEX_POINT('',#13960);
#4572=VERTEX_POINT('',#13964);
#4573=VERTEX_POINT('',#13968);
#4574=VERTEX_POINT('',#13974);
#4575=VERTEX_POINT('',#13978);
#4576=VERTEX_POINT('',#13982);
#4577=VERTEX_POINT('',#13986);
#4578=VERTEX_POINT('',#13994);
#4579=VERTEX_POINT('',#13995);
#4580=VERTEX_POINT('',#13997);
#4581=VERTEX_POINT('',#13999);
#4582=VERTEX_POINT('',#14003);
#4583=VERTEX_POINT('',#14005);
#4584=VERTEX_POINT('',#14009);
#4585=VERTEX_POINT('',#14011);
#4586=VERTEX_POINT('',#14015);
#4587=VERTEX_POINT('',#14017);
#4588=VERTEX_POINT('',#14021);
#4589=VERTEX_POINT('',#14023);
#4590=VERTEX_POINT('',#14027);
#4591=VERTEX_POINT('',#14029);
#4592=VERTEX_POINT('',#14033);
#4593=VERTEX_POINT('',#14035);
#4594=VERTEX_POINT('',#14045);
#4595=VERTEX_POINT('',#14046);
#4596=VERTEX_POINT('',#14048);
#4597=VERTEX_POINT('',#14050);
#4598=VERTEX_POINT('',#14054);
#4599=VERTEX_POINT('',#14056);
#4600=VERTEX_POINT('',#14060);
#4601=VERTEX_POINT('',#14062);
#4602=VERTEX_POINT('',#14066);
#4603=VERTEX_POINT('',#14068);
#4604=VERTEX_POINT('',#14072);
#4605=VERTEX_POINT('',#14074);
#4606=VERTEX_POINT('',#14078);
#4607=VERTEX_POINT('',#14080);
#4608=VERTEX_POINT('',#14084);
#4609=VERTEX_POINT('',#14086);
#4610=VERTEX_POINT('',#14099);
#4611=VERTEX_POINT('',#14101);
#4612=VERTEX_POINT('',#14105);
#4613=VERTEX_POINT('',#14109);
#4614=VERTEX_POINT('',#14112);
#4615=VERTEX_POINT('',#14118);
#4616=VERTEX_POINT('',#14121);
#4617=VERTEX_POINT('',#14125);
#4618=VERTEX_POINT('',#14129);
#4619=VERTEX_POINT('',#14133);
#4620=VERTEX_POINT('',#14136);
#4621=VERTEX_POINT('',#14140);
#4622=VERTEX_POINT('',#14144);
#4623=VERTEX_POINT('',#14149);
#4624=VERTEX_POINT('',#14150);
#4625=VERTEX_POINT('',#14152);
#4626=VERTEX_POINT('',#14154);
#4627=VERTEX_POINT('',#14158);
#4628=VERTEX_POINT('',#14160);
#4629=VERTEX_POINT('',#14164);
#4630=VERTEX_POINT('',#14166);
#4631=VERTEX_POINT('',#14170);
#4632=VERTEX_POINT('',#14172);
#4633=VERTEX_POINT('',#14176);
#4634=VERTEX_POINT('',#14178);
#4635=VERTEX_POINT('',#14188);
#4636=VERTEX_POINT('',#14190);
#4637=VERTEX_POINT('',#14194);
#4638=VERTEX_POINT('',#14198);
#4639=VERTEX_POINT('',#14201);
#4640=VERTEX_POINT('',#14207);
#4641=VERTEX_POINT('',#14210);
#4642=VERTEX_POINT('',#14214);
#4643=VERTEX_POINT('',#14218);
#4644=VERTEX_POINT('',#14222);
#4645=VERTEX_POINT('',#14225);
#4646=VERTEX_POINT('',#14229);
#4647=VERTEX_POINT('',#14233);
#4648=VERTEX_POINT('',#14238);
#4649=VERTEX_POINT('',#14239);
#4650=VERTEX_POINT('',#14241);
#4651=VERTEX_POINT('',#14243);
#4652=VERTEX_POINT('',#14247);
#4653=VERTEX_POINT('',#14249);
#4654=VERTEX_POINT('',#14253);
#4655=VERTEX_POINT('',#14255);
#4656=VERTEX_POINT('',#14259);
#4657=VERTEX_POINT('',#14261);
#4658=VERTEX_POINT('',#14265);
#4659=VERTEX_POINT('',#14267);
#4660=VERTEX_POINT('',#14314);
#4661=VERTEX_POINT('',#14316);
#4662=VERTEX_POINT('',#14320);
#4663=VERTEX_POINT('',#14322);
#4664=VERTEX_POINT('',#14329);
#4665=VERTEX_POINT('',#14332);
#4666=VERTEX_POINT('',#14336);
#4667=VERTEX_POINT('',#14340);
#4668=VERTEX_POINT('',#14344);
#4669=VERTEX_POINT('',#14347);
#4670=VERTEX_POINT('',#14351);
#4671=VERTEX_POINT('',#14355);
#4672=VERTEX_POINT('',#14360);
#4673=VERTEX_POINT('',#14361);
#4674=VERTEX_POINT('',#14363);
#4675=VERTEX_POINT('',#14365);
#4676=VERTEX_POINT('',#14369);
#4677=VERTEX_POINT('',#14371);
#4678=VERTEX_POINT('',#14375);
#4679=VERTEX_POINT('',#14377);
#4680=VERTEX_POINT('',#14381);
#4681=VERTEX_POINT('',#14383);
#4682=VERTEX_POINT('',#14387);
#4683=VERTEX_POINT('',#14389);
#4684=EDGE_CURVE('',#3938,#3938,#3782,.T.);
#4685=EDGE_CURVE('',#3938,#3939,#1840,.T.);
#4686=EDGE_CURVE('',#3939,#3939,#3783,.T.);
#4687=EDGE_CURVE('',#3940,#3940,#3784,.T.);
#4688=EDGE_CURVE('',#3940,#3941,#1841,.T.);
#4689=EDGE_CURVE('',#3941,#3941,#3785,.T.);
#4690=EDGE_CURVE('',#3942,#3942,#3786,.T.);
#4691=EDGE_CURVE('',#3942,#3943,#1842,.T.);
#4692=EDGE_CURVE('',#3943,#3943,#3787,.T.);
#4693=EDGE_CURVE('',#3944,#3944,#3788,.T.);
#4694=EDGE_CURVE('',#3944,#3945,#1843,.T.);
#4695=EDGE_CURVE('',#3945,#3945,#3789,.T.);
#4696=EDGE_CURVE('',#3946,#3946,#3790,.T.);
#4697=EDGE_CURVE('',#3946,#3947,#1844,.T.);
#4698=EDGE_CURVE('',#3947,#3947,#3791,.T.);
#4699=EDGE_CURVE('',#3948,#3948,#3792,.T.);
#4700=EDGE_CURVE('',#3948,#3949,#1845,.T.);
#4701=EDGE_CURVE('',#3949,#3949,#3793,.T.);
#4702=EDGE_CURVE('',#3950,#3950,#3794,.T.);
#4703=EDGE_CURVE('',#3950,#3951,#1846,.T.);
#4704=EDGE_CURVE('',#3951,#3951,#3795,.T.);
#4705=EDGE_CURVE('',#3952,#3952,#3796,.T.);
#4706=EDGE_CURVE('',#3952,#3953,#1847,.T.);
#4707=EDGE_CURVE('',#3953,#3953,#3797,.T.);
#4708=EDGE_CURVE('',#3954,#3954,#3798,.T.);
#4709=EDGE_CURVE('',#3954,#3955,#1848,.T.);
#4710=EDGE_CURVE('',#3955,#3955,#3799,.T.);
#4711=EDGE_CURVE('',#3956,#3956,#3800,.T.);
#4712=EDGE_CURVE('',#3956,#3957,#1849,.T.);
#4713=EDGE_CURVE('',#3957,#3957,#3801,.T.);
#4714=EDGE_CURVE('',#3958,#3958,#3802,.T.);
#4715=EDGE_CURVE('',#3958,#3959,#1850,.T.);
#4716=EDGE_CURVE('',#3959,#3959,#3803,.T.);
#4717=EDGE_CURVE('',#3960,#3960,#3804,.T.);
#4718=EDGE_CURVE('',#3960,#3961,#1851,.T.);
#4719=EDGE_CURVE('',#3961,#3961,#3805,.T.);
#4720=EDGE_CURVE('',#3962,#3962,#3806,.T.);
#4721=EDGE_CURVE('',#3962,#3963,#1852,.T.);
#4722=EDGE_CURVE('',#3963,#3963,#3807,.T.);
#4723=EDGE_CURVE('',#3964,#3964,#3808,.T.);
#4724=EDGE_CURVE('',#3964,#3965,#1853,.T.);
#4725=EDGE_CURVE('',#3965,#3965,#3809,.T.);
#4726=EDGE_CURVE('',#3966,#3967,#1854,.T.);
#4727=EDGE_CURVE('',#3967,#3968,#1855,.T.);
#4728=EDGE_CURVE('',#3969,#3968,#1856,.T.);
#4729=EDGE_CURVE('',#3966,#3969,#1857,.T.);
#4730=EDGE_CURVE('',#3970,#3966,#1858,.T.);
#4731=EDGE_CURVE('',#3971,#3969,#1859,.T.);
#4732=EDGE_CURVE('',#3970,#3971,#1860,.T.);
#4733=EDGE_CURVE('',#3972,#3970,#1861,.T.);
#4734=EDGE_CURVE('',#3973,#3971,#1862,.T.);
#4735=EDGE_CURVE('',#3972,#3973,#1863,.T.);
#4736=EDGE_CURVE('',#3967,#3972,#1864,.T.);
#4737=EDGE_CURVE('',#3968,#3973,#1865,.T.);
#4738=EDGE_CURVE('',#3974,#3974,#3810,.T.);
#4739=EDGE_CURVE('',#3974,#3975,#1866,.T.);
#4740=EDGE_CURVE('',#3975,#3975,#3811,.T.);
#4741=EDGE_CURVE('',#3976,#3976,#3812,.T.);
#4742=EDGE_CURVE('',#3977,#3977,#3813,.T.);
#4743=EDGE_CURVE('',#3977,#3978,#1867,.T.);
#4744=EDGE_CURVE('',#3978,#3978,#3814,.T.);
#4745=EDGE_CURVE('',#3979,#3979,#3815,.T.);
#4746=EDGE_CURVE('',#3980,#3980,#3816,.T.);
#4747=EDGE_CURVE('',#3980,#3976,#1868,.T.);
#4748=EDGE_CURVE('',#3981,#3981,#3817,.T.);
#4749=EDGE_CURVE('',#3981,#3979,#1869,.T.);
#4750=EDGE_CURVE('',#3982,#3983,#1870,.T.);
#4751=EDGE_CURVE('',#3983,#3984,#1871,.T.);
#4752=EDGE_CURVE('',#3985,#3984,#1872,.T.);
#4753=EDGE_CURVE('',#3982,#3985,#1873,.T.);
#4754=EDGE_CURVE('',#3986,#3982,#1874,.T.);
#4755=EDGE_CURVE('',#3987,#3985,#1875,.T.);
#4756=EDGE_CURVE('',#3986,#3987,#1876,.T.);
#4757=EDGE_CURVE('',#3988,#3986,#1877,.T.);
#4758=EDGE_CURVE('',#3989,#3987,#1878,.T.);
#4759=EDGE_CURVE('',#3988,#3989,#1879,.T.);
#4760=EDGE_CURVE('',#3983,#3988,#1880,.T.);
#4761=EDGE_CURVE('',#3984,#3989,#1881,.T.);
#4762=EDGE_CURVE('',#3990,#3991,#1882,.T.);
#4763=EDGE_CURVE('',#3991,#3992,#1883,.T.);
#4764=EDGE_CURVE('',#3993,#3992,#1884,.T.);
#4765=EDGE_CURVE('',#3990,#3993,#1885,.T.);
#4766=EDGE_CURVE('',#3994,#3990,#1886,.T.);
#4767=EDGE_CURVE('',#3995,#3993,#1887,.T.);
#4768=EDGE_CURVE('',#3994,#3995,#1888,.T.);
#4769=EDGE_CURVE('',#3996,#3994,#1889,.T.);
#4770=EDGE_CURVE('',#3997,#3995,#1890,.T.);
#4771=EDGE_CURVE('',#3996,#3997,#1891,.T.);
#4772=EDGE_CURVE('',#3991,#3996,#1892,.T.);
#4773=EDGE_CURVE('',#3992,#3997,#1893,.T.);
#4774=EDGE_CURVE('',#3998,#3998,#3818,.T.);
#4775=EDGE_CURVE('',#3998,#3999,#1894,.T.);
#4776=EDGE_CURVE('',#3999,#3999,#3819,.T.);
#4777=EDGE_CURVE('',#4000,#4000,#3820,.T.);
#4778=EDGE_CURVE('',#4001,#4001,#3821,.T.);
#4779=EDGE_CURVE('',#4001,#4002,#1895,.T.);
#4780=EDGE_CURVE('',#4002,#4002,#3822,.T.);
#4781=EDGE_CURVE('',#4003,#4003,#3823,.T.);
#4782=EDGE_CURVE('',#4004,#4004,#3824,.T.);
#4783=EDGE_CURVE('',#4004,#4000,#1896,.T.);
#4784=EDGE_CURVE('',#4005,#4005,#3825,.T.);
#4785=EDGE_CURVE('',#4005,#4003,#1897,.T.);
#4786=EDGE_CURVE('',#4006,#4007,#1898,.T.);
#4787=EDGE_CURVE('',#4007,#4008,#1899,.T.);
#4788=EDGE_CURVE('',#4009,#4008,#1900,.T.);
#4789=EDGE_CURVE('',#4006,#4009,#1901,.T.);
#4790=EDGE_CURVE('',#4010,#4006,#1902,.T.);
#4791=EDGE_CURVE('',#4011,#4009,#1903,.T.);
#4792=EDGE_CURVE('',#4010,#4011,#1904,.T.);
#4793=EDGE_CURVE('',#4012,#4010,#1905,.T.);
#4794=EDGE_CURVE('',#4013,#4011,#1906,.T.);
#4795=EDGE_CURVE('',#4012,#4013,#1907,.T.);
#4796=EDGE_CURVE('',#4007,#4012,#1908,.T.);
#4797=EDGE_CURVE('',#4008,#4013,#1909,.T.);
#4798=EDGE_CURVE('',#4014,#4015,#1910,.T.);
#4799=EDGE_CURVE('',#4015,#4016,#1911,.T.);
#4800=EDGE_CURVE('',#4017,#4016,#1912,.T.);
#4801=EDGE_CURVE('',#4014,#4017,#1913,.T.);
#4802=EDGE_CURVE('',#4018,#4014,#1914,.T.);
#4803=EDGE_CURVE('',#4019,#4017,#1915,.T.);
#4804=EDGE_CURVE('',#4018,#4019,#1916,.T.);
#4805=EDGE_CURVE('',#4020,#4018,#1917,.T.);
#4806=EDGE_CURVE('',#4021,#4019,#1918,.T.);
#4807=EDGE_CURVE('',#4020,#4021,#1919,.T.);
#4808=EDGE_CURVE('',#4015,#4020,#1920,.T.);
#4809=EDGE_CURVE('',#4016,#4021,#1921,.T.);
#4810=EDGE_CURVE('',#4022,#4023,#1922,.T.);
#4811=EDGE_CURVE('',#4022,#4024,#1923,.T.);
#4812=EDGE_CURVE('',#4025,#4024,#1924,.T.);
#4813=EDGE_CURVE('',#4023,#4025,#1925,.T.);
#4814=EDGE_CURVE('',#4026,#4022,#1926,.T.);
#4815=EDGE_CURVE('',#4027,#4026,#1927,.T.);
#4816=EDGE_CURVE('',#4024,#4027,#1928,.T.);
#4817=EDGE_CURVE('',#4023,#4028,#1929,.T.);
#4818=EDGE_CURVE('',#4029,#4025,#1930,.T.);
#4819=EDGE_CURVE('',#4028,#4029,#1931,.T.);
#4820=EDGE_CURVE('',#4026,#4028,#1932,.T.);
#4821=EDGE_CURVE('',#4030,#4031,#1933,.T.);
#4822=EDGE_CURVE('',#4030,#4032,#1934,.T.);
#4823=EDGE_CURVE('',#4033,#4032,#1935,.T.);
#4824=EDGE_CURVE('',#4031,#4033,#1936,.T.);
#4825=EDGE_CURVE('',#4034,#4030,#1937,.T.);
#4826=EDGE_CURVE('',#4035,#4034,#1938,.T.);
#4827=EDGE_CURVE('',#4032,#4035,#1939,.T.);
#4828=EDGE_CURVE('',#4031,#4036,#1940,.T.);
#4829=EDGE_CURVE('',#4037,#4033,#1941,.T.);
#4830=EDGE_CURVE('',#4036,#4037,#1942,.T.);
#4831=EDGE_CURVE('',#4034,#4036,#1943,.T.);
#4832=EDGE_CURVE('',#4038,#4039,#1944,.T.);
#4833=EDGE_CURVE('',#4038,#4040,#1945,.T.);
#4834=EDGE_CURVE('',#4041,#4040,#1946,.T.);
#4835=EDGE_CURVE('',#4039,#4041,#1947,.T.);
#4836=EDGE_CURVE('',#4042,#4038,#1948,.T.);
#4837=EDGE_CURVE('',#4043,#4042,#1949,.T.);
#4838=EDGE_CURVE('',#4040,#4043,#1950,.T.);
#4839=EDGE_CURVE('',#4039,#4044,#1951,.T.);
#4840=EDGE_CURVE('',#4045,#4041,#1952,.T.);
#4841=EDGE_CURVE('',#4044,#4045,#1953,.T.);
#4842=EDGE_CURVE('',#4042,#4044,#1954,.T.);
#4843=EDGE_CURVE('',#4046,#4047,#1955,.T.);
#4844=EDGE_CURVE('',#4046,#4048,#1956,.T.);
#4845=EDGE_CURVE('',#4049,#4048,#1957,.T.);
#4846=EDGE_CURVE('',#4047,#4049,#1958,.T.);
#4847=EDGE_CURVE('',#4050,#4046,#1959,.T.);
#4848=EDGE_CURVE('',#4051,#4050,#1960,.T.);
#4849=EDGE_CURVE('',#4048,#4051,#1961,.T.);
#4850=EDGE_CURVE('',#4047,#4052,#1962,.T.);
#4851=EDGE_CURVE('',#4053,#4049,#1963,.T.);
#4852=EDGE_CURVE('',#4052,#4053,#1964,.T.);
#4853=EDGE_CURVE('',#4050,#4052,#1965,.T.);
#4854=EDGE_CURVE('',#4054,#4055,#1966,.T.);
#4855=EDGE_CURVE('',#4054,#4056,#1967,.T.);
#4856=EDGE_CURVE('',#4057,#4056,#1968,.T.);
#4857=EDGE_CURVE('',#4055,#4057,#1969,.T.);
#4858=EDGE_CURVE('',#4058,#4054,#1970,.T.);
#4859=EDGE_CURVE('',#4059,#4058,#1971,.T.);
#4860=EDGE_CURVE('',#4056,#4059,#1972,.T.);
#4861=EDGE_CURVE('',#4055,#4060,#1973,.T.);
#4862=EDGE_CURVE('',#4061,#4057,#1974,.T.);
#4863=EDGE_CURVE('',#4060,#4061,#1975,.T.);
#4864=EDGE_CURVE('',#4058,#4060,#1976,.T.);
#4865=EDGE_CURVE('',#4062,#4063,#1977,.T.);
#4866=EDGE_CURVE('',#4062,#4064,#1978,.T.);
#4867=EDGE_CURVE('',#4065,#4064,#1979,.T.);
#4868=EDGE_CURVE('',#4063,#4065,#1980,.T.);
#4869=EDGE_CURVE('',#4066,#4062,#1981,.T.);
#4870=EDGE_CURVE('',#4067,#4066,#1982,.T.);
#4871=EDGE_CURVE('',#4064,#4067,#1983,.T.);
#4872=EDGE_CURVE('',#4063,#4068,#1984,.T.);
#4873=EDGE_CURVE('',#4069,#4065,#1985,.T.);
#4874=EDGE_CURVE('',#4068,#4069,#1986,.T.);
#4875=EDGE_CURVE('',#4066,#4068,#1987,.T.);
#4876=EDGE_CURVE('',#4070,#4071,#1988,.T.);
#4877=EDGE_CURVE('',#4070,#4072,#1989,.T.);
#4878=EDGE_CURVE('',#4073,#4072,#1990,.T.);
#4879=EDGE_CURVE('',#4071,#4073,#1991,.T.);
#4880=EDGE_CURVE('',#4074,#4070,#1992,.T.);
#4881=EDGE_CURVE('',#4075,#4074,#1993,.T.);
#4882=EDGE_CURVE('',#4072,#4075,#1994,.T.);
#4883=EDGE_CURVE('',#4071,#4076,#1995,.T.);
#4884=EDGE_CURVE('',#4077,#4073,#1996,.T.);
#4885=EDGE_CURVE('',#4076,#4077,#1997,.T.);
#4886=EDGE_CURVE('',#4074,#4076,#1998,.T.);
#4887=EDGE_CURVE('',#4078,#4079,#1999,.T.);
#4888=EDGE_CURVE('',#4078,#4080,#2000,.T.);
#4889=EDGE_CURVE('',#4081,#4080,#2001,.T.);
#4890=EDGE_CURVE('',#4079,#4081,#2002,.T.);
#4891=EDGE_CURVE('',#4082,#4078,#2003,.T.);
#4892=EDGE_CURVE('',#4083,#4082,#2004,.T.);
#4893=EDGE_CURVE('',#4080,#4083,#2005,.T.);
#4894=EDGE_CURVE('',#4079,#4084,#2006,.T.);
#4895=EDGE_CURVE('',#4085,#4081,#2007,.T.);
#4896=EDGE_CURVE('',#4084,#4085,#2008,.T.);
#4897=EDGE_CURVE('',#4082,#4084,#2009,.T.);
#4898=EDGE_CURVE('',#4086,#4087,#2010,.T.);
#4899=EDGE_CURVE('',#4086,#4088,#2011,.T.);
#4900=EDGE_CURVE('',#4089,#4088,#2012,.T.);
#4901=EDGE_CURVE('',#4087,#4089,#2013,.T.);
#4902=EDGE_CURVE('',#4090,#4086,#2014,.T.);
#4903=EDGE_CURVE('',#4091,#4090,#2015,.T.);
#4904=EDGE_CURVE('',#4088,#4091,#2016,.T.);
#4905=EDGE_CURVE('',#4087,#4092,#2017,.T.);
#4906=EDGE_CURVE('',#4093,#4089,#2018,.T.);
#4907=EDGE_CURVE('',#4092,#4093,#2019,.T.);
#4908=EDGE_CURVE('',#4090,#4092,#2020,.T.);
#4909=EDGE_CURVE('',#4094,#4095,#2021,.T.);
#4910=EDGE_CURVE('',#4094,#4096,#2022,.T.);
#4911=EDGE_CURVE('',#4097,#4096,#2023,.T.);
#4912=EDGE_CURVE('',#4095,#4097,#2024,.T.);
#4913=EDGE_CURVE('',#4098,#4094,#2025,.T.);
#4914=EDGE_CURVE('',#4099,#4098,#2026,.T.);
#4915=EDGE_CURVE('',#4096,#4099,#2027,.T.);
#4916=EDGE_CURVE('',#4095,#4100,#2028,.T.);
#4917=EDGE_CURVE('',#4101,#4097,#2029,.T.);
#4918=EDGE_CURVE('',#4100,#4101,#2030,.T.);
#4919=EDGE_CURVE('',#4098,#4100,#2031,.T.);
#4920=EDGE_CURVE('',#4102,#4103,#2032,.T.);
#4921=EDGE_CURVE('',#4102,#4104,#2033,.T.);
#4922=EDGE_CURVE('',#4105,#4104,#2034,.T.);
#4923=EDGE_CURVE('',#4103,#4105,#2035,.T.);
#4924=EDGE_CURVE('',#4106,#4102,#2036,.T.);
#4925=EDGE_CURVE('',#4107,#4106,#2037,.T.);
#4926=EDGE_CURVE('',#4104,#4107,#2038,.T.);
#4927=EDGE_CURVE('',#4103,#4108,#2039,.T.);
#4928=EDGE_CURVE('',#4109,#4105,#2040,.T.);
#4929=EDGE_CURVE('',#4108,#4109,#2041,.T.);
#4930=EDGE_CURVE('',#4106,#4108,#2042,.T.);
#4931=EDGE_CURVE('',#4110,#4111,#2043,.T.);
#4932=EDGE_CURVE('',#4110,#4112,#2044,.T.);
#4933=EDGE_CURVE('',#4113,#4112,#2045,.T.);
#4934=EDGE_CURVE('',#4111,#4113,#2046,.T.);
#4935=EDGE_CURVE('',#4114,#4110,#2047,.T.);
#4936=EDGE_CURVE('',#4115,#4114,#2048,.T.);
#4937=EDGE_CURVE('',#4112,#4115,#2049,.T.);
#4938=EDGE_CURVE('',#4111,#4116,#2050,.T.);
#4939=EDGE_CURVE('',#4117,#4113,#2051,.T.);
#4940=EDGE_CURVE('',#4116,#4117,#2052,.T.);
#4941=EDGE_CURVE('',#4114,#4116,#2053,.T.);
#4942=EDGE_CURVE('',#4118,#4119,#2054,.T.);
#4943=EDGE_CURVE('',#4118,#4120,#2055,.T.);
#4944=EDGE_CURVE('',#4121,#4120,#2056,.T.);
#4945=EDGE_CURVE('',#4119,#4121,#2057,.T.);
#4946=EDGE_CURVE('',#4122,#4118,#2058,.T.);
#4947=EDGE_CURVE('',#4123,#4122,#2059,.T.);
#4948=EDGE_CURVE('',#4120,#4123,#2060,.T.);
#4949=EDGE_CURVE('',#4119,#4124,#2061,.T.);
#4950=EDGE_CURVE('',#4125,#4121,#2062,.T.);
#4951=EDGE_CURVE('',#4124,#4125,#2063,.T.);
#4952=EDGE_CURVE('',#4122,#4124,#2064,.T.);
#4953=EDGE_CURVE('',#4126,#4127,#2065,.T.);
#4954=EDGE_CURVE('',#4126,#4128,#2066,.T.);
#4955=EDGE_CURVE('',#4129,#4128,#2067,.T.);
#4956=EDGE_CURVE('',#4127,#4129,#2068,.T.);
#4957=EDGE_CURVE('',#4130,#4126,#2069,.T.);
#4958=EDGE_CURVE('',#4131,#4130,#2070,.T.);
#4959=EDGE_CURVE('',#4128,#4131,#2071,.T.);
#4960=EDGE_CURVE('',#4127,#4132,#2072,.T.);
#4961=EDGE_CURVE('',#4133,#4129,#2073,.T.);
#4962=EDGE_CURVE('',#4132,#4133,#2074,.T.);
#4963=EDGE_CURVE('',#4130,#4132,#2075,.T.);
#4964=EDGE_CURVE('',#4134,#4135,#2076,.T.);
#4965=EDGE_CURVE('',#4134,#4136,#2077,.T.);
#4966=EDGE_CURVE('',#4137,#4136,#2078,.T.);
#4967=EDGE_CURVE('',#4135,#4137,#2079,.T.);
#4968=EDGE_CURVE('',#4138,#4134,#2080,.T.);
#4969=EDGE_CURVE('',#4139,#4138,#2081,.T.);
#4970=EDGE_CURVE('',#4136,#4139,#2082,.T.);
#4971=EDGE_CURVE('',#4135,#4140,#2083,.T.);
#4972=EDGE_CURVE('',#4141,#4137,#2084,.T.);
#4973=EDGE_CURVE('',#4140,#4141,#2085,.T.);
#4974=EDGE_CURVE('',#4138,#4140,#2086,.T.);
#4975=EDGE_CURVE('',#4142,#4143,#2087,.T.);
#4976=EDGE_CURVE('',#4142,#4144,#2088,.T.);
#4977=EDGE_CURVE('',#4145,#4144,#2089,.T.);
#4978=EDGE_CURVE('',#4143,#4145,#2090,.T.);
#4979=EDGE_CURVE('',#4146,#4142,#2091,.T.);
#4980=EDGE_CURVE('',#4147,#4146,#2092,.T.);
#4981=EDGE_CURVE('',#4144,#4147,#2093,.T.);
#4982=EDGE_CURVE('',#4143,#4148,#2094,.T.);
#4983=EDGE_CURVE('',#4149,#4145,#2095,.T.);
#4984=EDGE_CURVE('',#4148,#4149,#2096,.T.);
#4985=EDGE_CURVE('',#4146,#4148,#2097,.T.);
#4986=EDGE_CURVE('',#4150,#4151,#2098,.T.);
#4987=EDGE_CURVE('',#4150,#4152,#2099,.T.);
#4988=EDGE_CURVE('',#4153,#4152,#2100,.T.);
#4989=EDGE_CURVE('',#4151,#4153,#2101,.T.);
#4990=EDGE_CURVE('',#4154,#4150,#2102,.T.);
#4991=EDGE_CURVE('',#4155,#4154,#2103,.T.);
#4992=EDGE_CURVE('',#4152,#4155,#2104,.T.);
#4993=EDGE_CURVE('',#4151,#4156,#2105,.T.);
#4994=EDGE_CURVE('',#4157,#4153,#2106,.T.);
#4995=EDGE_CURVE('',#4156,#4157,#2107,.T.);
#4996=EDGE_CURVE('',#4154,#4156,#2108,.T.);
#4997=EDGE_CURVE('',#4158,#4159,#2109,.T.);
#4998=EDGE_CURVE('',#4158,#4160,#2110,.T.);
#4999=EDGE_CURVE('',#4161,#4160,#2111,.T.);
#5000=EDGE_CURVE('',#4159,#4161,#2112,.T.);
#5001=EDGE_CURVE('',#4162,#4158,#2113,.T.);
#5002=EDGE_CURVE('',#4163,#4162,#2114,.T.);
#5003=EDGE_CURVE('',#4160,#4163,#2115,.T.);
#5004=EDGE_CURVE('',#4159,#4164,#2116,.T.);
#5005=EDGE_CURVE('',#4165,#4161,#2117,.T.);
#5006=EDGE_CURVE('',#4164,#4165,#2118,.T.);
#5007=EDGE_CURVE('',#4162,#4164,#2119,.T.);
#5008=EDGE_CURVE('',#4166,#4167,#2120,.T.);
#5009=EDGE_CURVE('',#4166,#4168,#2121,.T.);
#5010=EDGE_CURVE('',#4169,#4168,#2122,.T.);
#5011=EDGE_CURVE('',#4167,#4169,#2123,.T.);
#5012=EDGE_CURVE('',#4170,#4166,#2124,.T.);
#5013=EDGE_CURVE('',#4171,#4170,#2125,.T.);
#5014=EDGE_CURVE('',#4168,#4171,#2126,.T.);
#5015=EDGE_CURVE('',#4167,#4172,#2127,.T.);
#5016=EDGE_CURVE('',#4173,#4169,#2128,.T.);
#5017=EDGE_CURVE('',#4172,#4173,#2129,.T.);
#5018=EDGE_CURVE('',#4170,#4172,#2130,.T.);
#5019=EDGE_CURVE('',#4174,#4175,#2131,.T.);
#5020=EDGE_CURVE('',#4174,#4176,#2132,.T.);
#5021=EDGE_CURVE('',#4177,#4176,#2133,.T.);
#5022=EDGE_CURVE('',#4175,#4177,#2134,.T.);
#5023=EDGE_CURVE('',#4178,#4174,#2135,.T.);
#5024=EDGE_CURVE('',#4179,#4178,#2136,.T.);
#5025=EDGE_CURVE('',#4176,#4179,#2137,.T.);
#5026=EDGE_CURVE('',#4175,#4180,#2138,.T.);
#5027=EDGE_CURVE('',#4181,#4177,#2139,.T.);
#5028=EDGE_CURVE('',#4180,#4181,#2140,.T.);
#5029=EDGE_CURVE('',#4178,#4180,#2141,.T.);
#5030=EDGE_CURVE('',#4182,#4183,#2142,.T.);
#5031=EDGE_CURVE('',#4182,#4184,#2143,.T.);
#5032=EDGE_CURVE('',#4185,#4184,#2144,.T.);
#5033=EDGE_CURVE('',#4183,#4185,#2145,.T.);
#5034=EDGE_CURVE('',#4186,#4182,#2146,.T.);
#5035=EDGE_CURVE('',#4187,#4186,#2147,.T.);
#5036=EDGE_CURVE('',#4184,#4187,#2148,.T.);
#5037=EDGE_CURVE('',#4183,#4188,#2149,.T.);
#5038=EDGE_CURVE('',#4189,#4185,#2150,.T.);
#5039=EDGE_CURVE('',#4188,#4189,#2151,.T.);
#5040=EDGE_CURVE('',#4186,#4188,#2152,.T.);
#5041=EDGE_CURVE('',#4190,#4191,#2153,.T.);
#5042=EDGE_CURVE('',#4190,#4192,#2154,.T.);
#5043=EDGE_CURVE('',#4193,#4192,#2155,.T.);
#5044=EDGE_CURVE('',#4191,#4193,#2156,.T.);
#5045=EDGE_CURVE('',#4194,#4190,#2157,.T.);
#5046=EDGE_CURVE('',#4195,#4194,#2158,.T.);
#5047=EDGE_CURVE('',#4192,#4195,#2159,.T.);
#5048=EDGE_CURVE('',#4191,#4196,#2160,.T.);
#5049=EDGE_CURVE('',#4197,#4193,#2161,.T.);
#5050=EDGE_CURVE('',#4196,#4197,#2162,.T.);
#5051=EDGE_CURVE('',#4194,#4196,#2163,.T.);
#5052=EDGE_CURVE('',#4198,#4199,#2164,.T.);
#5053=EDGE_CURVE('',#4198,#4200,#2165,.T.);
#5054=EDGE_CURVE('',#4201,#4200,#2166,.T.);
#5055=EDGE_CURVE('',#4199,#4201,#2167,.T.);
#5056=EDGE_CURVE('',#4202,#4198,#2168,.T.);
#5057=EDGE_CURVE('',#4203,#4202,#2169,.T.);
#5058=EDGE_CURVE('',#4200,#4203,#2170,.T.);
#5059=EDGE_CURVE('',#4199,#4204,#2171,.T.);
#5060=EDGE_CURVE('',#4205,#4201,#2172,.T.);
#5061=EDGE_CURVE('',#4204,#4205,#2173,.T.);
#5062=EDGE_CURVE('',#4202,#4204,#2174,.T.);
#5063=EDGE_CURVE('',#4206,#4207,#2175,.T.);
#5064=EDGE_CURVE('',#4206,#4208,#2176,.T.);
#5065=EDGE_CURVE('',#4209,#4208,#2177,.T.);
#5066=EDGE_CURVE('',#4207,#4209,#2178,.T.);
#5067=EDGE_CURVE('',#4210,#4206,#2179,.T.);
#5068=EDGE_CURVE('',#4211,#4210,#2180,.T.);
#5069=EDGE_CURVE('',#4208,#4211,#2181,.T.);
#5070=EDGE_CURVE('',#4207,#4212,#2182,.T.);
#5071=EDGE_CURVE('',#4213,#4209,#2183,.T.);
#5072=EDGE_CURVE('',#4212,#4213,#2184,.T.);
#5073=EDGE_CURVE('',#4210,#4212,#2185,.T.);
#5074=EDGE_CURVE('',#4214,#4215,#2186,.T.);
#5075=EDGE_CURVE('',#4214,#4216,#2187,.T.);
#5076=EDGE_CURVE('',#4217,#4216,#2188,.T.);
#5077=EDGE_CURVE('',#4215,#4217,#2189,.T.);
#5078=EDGE_CURVE('',#4218,#4214,#2190,.T.);
#5079=EDGE_CURVE('',#4219,#4218,#2191,.T.);
#5080=EDGE_CURVE('',#4216,#4219,#2192,.T.);
#5081=EDGE_CURVE('',#4215,#4220,#2193,.T.);
#5082=EDGE_CURVE('',#4221,#4217,#2194,.T.);
#5083=EDGE_CURVE('',#4220,#4221,#2195,.T.);
#5084=EDGE_CURVE('',#4218,#4220,#2196,.T.);
#5085=EDGE_CURVE('',#4222,#4223,#2197,.T.);
#5086=EDGE_CURVE('',#4222,#4224,#2198,.T.);
#5087=EDGE_CURVE('',#4225,#4224,#2199,.T.);
#5088=EDGE_CURVE('',#4223,#4225,#2200,.T.);
#5089=EDGE_CURVE('',#4226,#4222,#2201,.T.);
#5090=EDGE_CURVE('',#4227,#4226,#2202,.T.);
#5091=EDGE_CURVE('',#4224,#4227,#2203,.T.);
#5092=EDGE_CURVE('',#4223,#4228,#2204,.T.);
#5093=EDGE_CURVE('',#4229,#4225,#2205,.T.);
#5094=EDGE_CURVE('',#4228,#4229,#2206,.T.);
#5095=EDGE_CURVE('',#4226,#4228,#2207,.T.);
#5096=EDGE_CURVE('',#4230,#4231,#2208,.T.);
#5097=EDGE_CURVE('',#4230,#4232,#2209,.T.);
#5098=EDGE_CURVE('',#4233,#4232,#2210,.T.);
#5099=EDGE_CURVE('',#4231,#4233,#2211,.T.);
#5100=EDGE_CURVE('',#4234,#4230,#2212,.T.);
#5101=EDGE_CURVE('',#4235,#4234,#2213,.T.);
#5102=EDGE_CURVE('',#4232,#4235,#2214,.T.);
#5103=EDGE_CURVE('',#4231,#4236,#2215,.T.);
#5104=EDGE_CURVE('',#4237,#4233,#2216,.T.);
#5105=EDGE_CURVE('',#4236,#4237,#2217,.T.);
#5106=EDGE_CURVE('',#4234,#4236,#2218,.T.);
#5107=EDGE_CURVE('',#4238,#4239,#2219,.T.);
#5108=EDGE_CURVE('',#4238,#4240,#2220,.T.);
#5109=EDGE_CURVE('',#4241,#4240,#2221,.T.);
#5110=EDGE_CURVE('',#4239,#4241,#2222,.T.);
#5111=EDGE_CURVE('',#4242,#4238,#2223,.T.);
#5112=EDGE_CURVE('',#4243,#4242,#2224,.T.);
#5113=EDGE_CURVE('',#4240,#4243,#2225,.T.);
#5114=EDGE_CURVE('',#4239,#4244,#2226,.T.);
#5115=EDGE_CURVE('',#4245,#4241,#2227,.T.);
#5116=EDGE_CURVE('',#4244,#4245,#2228,.T.);
#5117=EDGE_CURVE('',#4242,#4244,#2229,.T.);
#5118=EDGE_CURVE('',#4246,#4247,#2230,.T.);
#5119=EDGE_CURVE('',#4246,#4248,#2231,.T.);
#5120=EDGE_CURVE('',#4249,#4248,#2232,.T.);
#5121=EDGE_CURVE('',#4247,#4249,#2233,.T.);
#5122=EDGE_CURVE('',#4250,#4246,#2234,.T.);
#5123=EDGE_CURVE('',#4251,#4250,#2235,.T.);
#5124=EDGE_CURVE('',#4248,#4251,#2236,.T.);
#5125=EDGE_CURVE('',#4247,#4252,#2237,.T.);
#5126=EDGE_CURVE('',#4253,#4249,#2238,.T.);
#5127=EDGE_CURVE('',#4252,#4253,#2239,.T.);
#5128=EDGE_CURVE('',#4250,#4252,#2240,.T.);
#5129=EDGE_CURVE('',#4027,#4253,#2241,.T.);
#5130=EDGE_CURVE('',#4251,#4254,#2242,.T.);
#5131=EDGE_CURVE('',#4254,#4255,#2243,.T.);
#5132=EDGE_CURVE('',#4255,#4256,#2244,.T.);
#5133=EDGE_CURVE('',#4256,#4257,#2245,.T.);
#5134=EDGE_CURVE('',#4257,#4197,#2246,.T.);
#5135=EDGE_CURVE('',#4195,#4141,#2247,.T.);
#5136=EDGE_CURVE('',#4139,#4133,#2248,.T.);
#5137=EDGE_CURVE('',#4131,#4149,#2249,.T.);
#5138=EDGE_CURVE('',#4147,#4125,#2250,.T.);
#5139=EDGE_CURVE('',#4123,#4157,#2251,.T.);
#5140=EDGE_CURVE('',#4155,#4117,#2252,.T.);
#5141=EDGE_CURVE('',#4115,#4165,#2253,.T.);
#5142=EDGE_CURVE('',#4163,#4109,#2254,.T.);
#5143=EDGE_CURVE('',#4107,#4173,#2255,.T.);
#5144=EDGE_CURVE('',#4171,#4101,#2256,.T.);
#5145=EDGE_CURVE('',#4099,#4181,#2257,.T.);
#5146=EDGE_CURVE('',#4179,#4093,#2258,.T.);
#5147=EDGE_CURVE('',#4091,#4189,#2259,.T.);
#5148=EDGE_CURVE('',#4187,#4085,#2260,.T.);
#5149=EDGE_CURVE('',#4083,#4077,#2261,.T.);
#5150=EDGE_CURVE('',#4075,#4205,#2262,.T.);
#5151=EDGE_CURVE('',#4203,#4069,#2263,.T.);
#5152=EDGE_CURVE('',#4067,#4213,#2264,.T.);
#5153=EDGE_CURVE('',#4211,#4061,#2265,.T.);
#5154=EDGE_CURVE('',#4059,#4221,#2266,.T.);
#5155=EDGE_CURVE('',#4219,#4053,#2267,.T.);
#5156=EDGE_CURVE('',#4051,#4229,#2268,.T.);
#5157=EDGE_CURVE('',#4227,#4045,#2269,.T.);
#5158=EDGE_CURVE('',#4043,#4237,#2270,.T.);
#5159=EDGE_CURVE('',#4235,#4037,#2271,.T.);
#5160=EDGE_CURVE('',#4035,#4245,#2272,.T.);
#5161=EDGE_CURVE('',#4243,#4029,#2273,.T.);
#5162=EDGE_CURVE('',#4258,#4258,#3826,.T.);
#5163=EDGE_CURVE('',#4259,#4259,#3827,.T.);
#5164=EDGE_CURVE('',#4260,#4260,#3828,.T.);
#5165=EDGE_CURVE('',#4260,#4259,#2274,.T.);
#5166=EDGE_CURVE('',#4261,#4261,#3829,.T.);
#5167=EDGE_CURVE('',#4261,#4258,#2275,.T.);
#5168=EDGE_CURVE('',#4262,#4263,#2276,.T.);
#5169=EDGE_CURVE('',#4263,#4256,#2277,.T.);
#5170=EDGE_CURVE('',#4262,#4255,#2278,.T.);
#5171=EDGE_CURVE('',#4264,#4262,#2279,.T.);
#5172=EDGE_CURVE('',#4264,#4254,#2280,.T.);
#5173=EDGE_CURVE('',#4265,#4257,#2281,.T.);
#5174=EDGE_CURVE('',#4265,#4264,#2282,.T.);
#5175=EDGE_CURVE('',#4263,#4265,#2283,.T.);
#5176=EDGE_CURVE('',#4266,#4267,#2284,.T.);
#5177=EDGE_CURVE('',#4267,#4268,#2285,.T.);
#5178=EDGE_CURVE('',#4269,#4268,#2286,.T.);
#5179=EDGE_CURVE('',#4266,#4269,#2287,.T.);
#5180=EDGE_CURVE('',#4270,#4266,#2288,.T.);
#5181=EDGE_CURVE('',#4271,#4269,#2289,.T.);
#5182=EDGE_CURVE('',#4270,#4271,#2290,.T.);
#5183=EDGE_CURVE('',#4272,#4270,#2291,.T.);
#5184=EDGE_CURVE('',#4273,#4271,#2292,.T.);
#5185=EDGE_CURVE('',#4272,#4273,#2293,.T.);
#5186=EDGE_CURVE('',#4267,#4272,#2294,.T.);
#5187=EDGE_CURVE('',#4268,#4273,#2295,.T.);
#5188=EDGE_CURVE('',#4274,#4275,#2296,.T.);
#5189=EDGE_CURVE('',#4275,#4276,#2297,.T.);
#5190=EDGE_CURVE('',#4277,#4276,#2298,.T.);
#5191=EDGE_CURVE('',#4274,#4277,#2299,.T.);
#5192=EDGE_CURVE('',#4278,#4274,#2300,.T.);
#5193=EDGE_CURVE('',#4279,#4277,#2301,.T.);
#5194=EDGE_CURVE('',#4278,#4279,#2302,.T.);
#5195=EDGE_CURVE('',#4280,#4278,#2303,.T.);
#5196=EDGE_CURVE('',#4281,#4279,#2304,.T.);
#5197=EDGE_CURVE('',#4280,#4281,#2305,.T.);
#5198=EDGE_CURVE('',#4275,#4280,#2306,.T.);
#5199=EDGE_CURVE('',#4276,#4281,#2307,.T.);
#5200=EDGE_CURVE('',#4282,#4283,#2308,.T.);
#5201=EDGE_CURVE('',#4283,#4284,#2309,.T.);
#5202=EDGE_CURVE('',#4285,#4284,#2310,.T.);
#5203=EDGE_CURVE('',#4282,#4285,#2311,.T.);
#5204=EDGE_CURVE('',#4286,#4282,#2312,.T.);
#5205=EDGE_CURVE('',#4287,#4285,#2313,.T.);
#5206=EDGE_CURVE('',#4286,#4287,#2314,.T.);
#5207=EDGE_CURVE('',#4288,#4286,#2315,.T.);
#5208=EDGE_CURVE('',#4289,#4287,#2316,.T.);
#5209=EDGE_CURVE('',#4288,#4289,#2317,.T.);
#5210=EDGE_CURVE('',#4283,#4288,#2318,.T.);
#5211=EDGE_CURVE('',#4284,#4289,#2319,.T.);
#5212=EDGE_CURVE('',#4290,#4291,#2320,.T.);
#5213=EDGE_CURVE('',#4291,#4292,#2321,.T.);
#5214=EDGE_CURVE('',#4293,#4292,#2322,.T.);
#5215=EDGE_CURVE('',#4290,#4293,#2323,.T.);
#5216=EDGE_CURVE('',#4294,#4290,#2324,.T.);
#5217=EDGE_CURVE('',#4295,#4293,#2325,.T.);
#5218=EDGE_CURVE('',#4294,#4295,#2326,.T.);
#5219=EDGE_CURVE('',#4296,#4294,#2327,.T.);
#5220=EDGE_CURVE('',#4297,#4295,#2328,.T.);
#5221=EDGE_CURVE('',#4296,#4297,#2329,.T.);
#5222=EDGE_CURVE('',#4291,#4296,#2330,.T.);
#5223=EDGE_CURVE('',#4292,#4297,#2331,.T.);
#5224=EDGE_CURVE('',#4298,#4298,#3830,.T.);
#5225=EDGE_CURVE('',#4298,#4299,#2332,.T.);
#5226=EDGE_CURVE('',#4299,#4299,#3831,.T.);
#5227=EDGE_CURVE('',#4300,#4300,#3832,.T.);
#5228=EDGE_CURVE('',#4301,#4301,#3833,.T.);
#5229=EDGE_CURVE('',#4301,#4302,#2333,.T.);
#5230=EDGE_CURVE('',#4302,#4302,#3834,.T.);
#5231=EDGE_CURVE('',#4303,#4303,#3835,.T.);
#5232=EDGE_CURVE('',#4304,#4304,#3836,.T.);
#5233=EDGE_CURVE('',#4304,#4305,#2334,.T.);
#5234=EDGE_CURVE('',#4305,#4305,#3837,.T.);
#5235=EDGE_CURVE('',#4306,#4306,#3838,.T.);
#5236=EDGE_CURVE('',#4307,#4307,#3839,.T.);
#5237=EDGE_CURVE('',#4307,#4308,#2335,.T.);
#5238=EDGE_CURVE('',#4308,#4308,#3840,.T.);
#5239=EDGE_CURVE('',#4309,#4309,#3841,.T.);
#5240=EDGE_CURVE('',#4310,#4310,#3842,.T.);
#5241=EDGE_CURVE('',#4310,#4300,#2336,.T.);
#5242=EDGE_CURVE('',#4311,#4311,#3843,.T.);
#5243=EDGE_CURVE('',#4311,#4303,#2337,.T.);
#5244=EDGE_CURVE('',#4312,#4312,#3844,.T.);
#5245=EDGE_CURVE('',#4312,#4306,#2338,.T.);
#5246=EDGE_CURVE('',#4313,#4313,#3845,.T.);
#5247=EDGE_CURVE('',#4313,#4309,#2339,.T.);
#5248=EDGE_CURVE('',#4314,#4315,#2340,.T.);
#5249=EDGE_CURVE('',#4315,#4316,#2341,.T.);
#5250=EDGE_CURVE('',#4317,#4316,#2342,.T.);
#5251=EDGE_CURVE('',#4314,#4317,#2343,.T.);
#5252=EDGE_CURVE('',#4318,#4314,#2344,.T.);
#5253=EDGE_CURVE('',#4319,#4317,#2345,.T.);
#5254=EDGE_CURVE('',#4318,#4319,#2346,.T.);
#5255=EDGE_CURVE('',#4320,#4318,#2347,.T.);
#5256=EDGE_CURVE('',#4321,#4319,#2348,.T.);
#5257=EDGE_CURVE('',#4320,#4321,#2349,.T.);
#5258=EDGE_CURVE('',#4322,#4320,#2350,.T.);
#5259=EDGE_CURVE('',#4323,#4321,#2351,.T.);
#5260=EDGE_CURVE('',#4322,#4323,#2352,.T.);
#5261=EDGE_CURVE('',#4324,#4322,#2353,.T.);
#5262=EDGE_CURVE('',#4325,#4323,#2354,.T.);
#5263=EDGE_CURVE('',#4324,#4325,#2355,.T.);
#5264=EDGE_CURVE('',#4326,#4324,#2356,.T.);
#5265=EDGE_CURVE('',#4327,#4325,#2357,.T.);
#5266=EDGE_CURVE('',#4326,#4327,#2358,.T.);
#5267=EDGE_CURVE('',#4328,#4326,#2359,.T.);
#5268=EDGE_CURVE('',#4329,#4327,#2360,.T.);
#5269=EDGE_CURVE('',#4328,#4329,#2361,.T.);
#5270=EDGE_CURVE('',#4330,#4328,#2362,.T.);
#5271=EDGE_CURVE('',#4331,#4329,#2363,.T.);
#5272=EDGE_CURVE('',#4330,#4331,#2364,.T.);
#5273=EDGE_CURVE('',#4332,#4330,#2365,.T.);
#5274=EDGE_CURVE('',#4333,#4331,#2366,.T.);
#5275=EDGE_CURVE('',#4332,#4333,#2367,.T.);
#5276=EDGE_CURVE('',#4334,#4332,#2368,.T.);
#5277=EDGE_CURVE('',#4335,#4333,#2369,.T.);
#5278=EDGE_CURVE('',#4334,#4335,#2370,.T.);
#5279=EDGE_CURVE('',#4336,#4334,#2371,.T.);
#5280=EDGE_CURVE('',#4337,#4335,#2372,.T.);
#5281=EDGE_CURVE('',#4336,#4337,#2373,.T.);
#5282=EDGE_CURVE('',#4315,#4336,#2374,.T.);
#5283=EDGE_CURVE('',#4316,#4337,#2375,.T.);
#5284=EDGE_CURVE('',#4338,#4339,#2376,.T.);
#5285=EDGE_CURVE('',#4338,#4340,#2377,.T.);
#5286=EDGE_CURVE('',#4341,#4340,#2378,.T.);
#5287=EDGE_CURVE('',#4339,#4341,#2379,.T.);
#5288=EDGE_CURVE('',#4342,#4338,#2380,.T.);
#5289=EDGE_CURVE('',#4342,#4343,#2381,.T.);
#5290=EDGE_CURVE('',#4340,#4343,#2382,.T.);
#5291=EDGE_CURVE('',#4344,#4342,#2383,.T.);
#5292=EDGE_CURVE('',#4344,#4345,#2384,.T.);
#5293=EDGE_CURVE('',#4343,#4345,#2385,.T.);
#5294=EDGE_CURVE('',#4346,#4344,#2386,.T.);
#5295=EDGE_CURVE('',#4346,#4347,#2387,.T.);
#5296=EDGE_CURVE('',#4345,#4347,#2388,.T.);
#5297=EDGE_CURVE('',#4348,#4346,#2389,.T.);
#5298=EDGE_CURVE('',#4348,#4349,#2390,.T.);
#5299=EDGE_CURVE('',#4347,#4349,#2391,.T.);
#5300=EDGE_CURVE('',#4350,#4348,#2392,.T.);
#5301=EDGE_CURVE('',#4350,#4351,#2393,.T.);
#5302=EDGE_CURVE('',#4349,#4351,#2394,.T.);
#5303=EDGE_CURVE('',#4352,#4350,#2395,.T.);
#5304=EDGE_CURVE('',#4352,#4353,#2396,.T.);
#5305=EDGE_CURVE('',#4351,#4353,#2397,.T.);
#5306=EDGE_CURVE('',#4354,#4352,#2398,.T.);
#5307=EDGE_CURVE('',#4354,#4355,#2399,.T.);
#5308=EDGE_CURVE('',#4353,#4355,#2400,.T.);
#5309=EDGE_CURVE('',#4356,#4354,#2401,.T.);
#5310=EDGE_CURVE('',#4357,#4356,#2402,.T.);
#5311=EDGE_CURVE('',#4355,#4357,#2403,.T.);
#5312=EDGE_CURVE('',#4358,#4359,#2404,.T.);
#5313=EDGE_CURVE('',#4358,#4360,#2405,.T.);
#5314=EDGE_CURVE('',#4361,#4360,#2406,.T.);
#5315=EDGE_CURVE('',#4359,#4361,#2407,.T.);
#5316=EDGE_CURVE('',#4362,#4358,#2408,.T.);
#5317=EDGE_CURVE('',#4362,#4363,#2409,.T.);
#5318=EDGE_CURVE('',#4360,#4363,#2410,.T.);
#5319=EDGE_CURVE('',#4364,#4362,#2411,.T.);
#5320=EDGE_CURVE('',#4364,#4365,#2412,.T.);
#5321=EDGE_CURVE('',#4363,#4365,#2413,.T.);
#5322=EDGE_CURVE('',#4366,#4364,#2414,.T.);
#5323=EDGE_CURVE('',#4366,#4367,#2415,.T.);
#5324=EDGE_CURVE('',#4365,#4367,#2416,.T.);
#5325=EDGE_CURVE('',#4368,#4366,#2417,.T.);
#5326=EDGE_CURVE('',#4368,#4369,#2418,.T.);
#5327=EDGE_CURVE('',#4367,#4369,#2419,.T.);
#5328=EDGE_CURVE('',#4370,#4368,#2420,.T.);
#5329=EDGE_CURVE('',#4370,#4371,#2421,.T.);
#5330=EDGE_CURVE('',#4369,#4371,#2422,.T.);
#5331=EDGE_CURVE('',#4372,#4370,#2423,.T.);
#5332=EDGE_CURVE('',#4372,#4373,#2424,.T.);
#5333=EDGE_CURVE('',#4371,#4373,#2425,.T.);
#5334=EDGE_CURVE('',#4374,#4372,#2426,.T.);
#5335=EDGE_CURVE('',#4374,#4375,#2427,.T.);
#5336=EDGE_CURVE('',#4373,#4375,#2428,.T.);
#5337=EDGE_CURVE('',#4376,#4374,#2429,.T.);
#5338=EDGE_CURVE('',#4377,#4376,#2430,.T.);
#5339=EDGE_CURVE('',#4375,#4377,#2431,.T.);
#5340=EDGE_CURVE('',#4378,#4379,#2432,.T.);
#5341=EDGE_CURVE('',#4378,#4380,#2433,.T.);
#5342=EDGE_CURVE('',#4381,#4380,#2434,.T.);
#5343=EDGE_CURVE('',#4379,#4381,#2435,.T.);
#5344=EDGE_CURVE('',#4382,#4378,#2436,.T.);
#5345=EDGE_CURVE('',#4382,#4383,#2437,.T.);
#5346=EDGE_CURVE('',#4380,#4383,#2438,.T.);
#5347=EDGE_CURVE('',#4384,#4382,#2439,.T.);
#5348=EDGE_CURVE('',#4384,#4385,#2440,.T.);
#5349=EDGE_CURVE('',#4383,#4385,#2441,.T.);
#5350=EDGE_CURVE('',#4386,#4384,#2442,.T.);
#5351=EDGE_CURVE('',#4386,#4387,#2443,.T.);
#5352=EDGE_CURVE('',#4385,#4387,#2444,.T.);
#5353=EDGE_CURVE('',#4388,#4386,#2445,.T.);
#5354=EDGE_CURVE('',#4388,#4389,#2446,.T.);
#5355=EDGE_CURVE('',#4387,#4389,#2447,.T.);
#5356=EDGE_CURVE('',#4390,#4388,#2448,.T.);
#5357=EDGE_CURVE('',#4390,#4391,#2449,.T.);
#5358=EDGE_CURVE('',#4389,#4391,#2450,.T.);
#5359=EDGE_CURVE('',#4392,#4390,#2451,.T.);
#5360=EDGE_CURVE('',#4392,#4393,#2452,.T.);
#5361=EDGE_CURVE('',#4391,#4393,#2453,.T.);
#5362=EDGE_CURVE('',#4394,#4392,#2454,.T.);
#5363=EDGE_CURVE('',#4394,#4395,#2455,.T.);
#5364=EDGE_CURVE('',#4393,#4395,#2456,.T.);
#5365=EDGE_CURVE('',#4396,#4394,#2457,.T.);
#5366=EDGE_CURVE('',#4397,#4396,#2458,.T.);
#5367=EDGE_CURVE('',#4395,#4397,#2459,.T.);
#5368=EDGE_CURVE('',#4398,#4399,#2460,.T.);
#5369=EDGE_CURVE('',#4398,#4400,#2461,.T.);
#5370=EDGE_CURVE('',#4401,#4400,#2462,.T.);
#5371=EDGE_CURVE('',#4399,#4401,#2463,.T.);
#5372=EDGE_CURVE('',#4402,#4398,#2464,.T.);
#5373=EDGE_CURVE('',#4402,#4403,#2465,.T.);
#5374=EDGE_CURVE('',#4400,#4403,#2466,.T.);
#5375=EDGE_CURVE('',#4404,#4402,#2467,.T.);
#5376=EDGE_CURVE('',#4404,#4405,#2468,.T.);
#5377=EDGE_CURVE('',#4403,#4405,#2469,.T.);
#5378=EDGE_CURVE('',#4406,#4404,#2470,.T.);
#5379=EDGE_CURVE('',#4406,#4407,#2471,.T.);
#5380=EDGE_CURVE('',#4405,#4407,#2472,.T.);
#5381=EDGE_CURVE('',#4408,#4406,#2473,.T.);
#5382=EDGE_CURVE('',#4408,#4409,#2474,.T.);
#5383=EDGE_CURVE('',#4407,#4409,#2475,.T.);
#5384=EDGE_CURVE('',#4410,#4408,#2476,.T.);
#5385=EDGE_CURVE('',#4410,#4411,#2477,.T.);
#5386=EDGE_CURVE('',#4409,#4411,#2478,.T.);
#5387=EDGE_CURVE('',#4412,#4410,#2479,.T.);
#5388=EDGE_CURVE('',#4412,#4413,#2480,.T.);
#5389=EDGE_CURVE('',#4411,#4413,#2481,.T.);
#5390=EDGE_CURVE('',#4414,#4412,#2482,.T.);
#5391=EDGE_CURVE('',#4414,#4415,#2483,.T.);
#5392=EDGE_CURVE('',#4413,#4415,#2484,.T.);
#5393=EDGE_CURVE('',#4416,#4414,#2485,.T.);
#5394=EDGE_CURVE('',#4417,#4416,#2486,.T.);
#5395=EDGE_CURVE('',#4415,#4417,#2487,.T.);
#5396=EDGE_CURVE('',#4418,#4418,#3846,.T.);
#5397=EDGE_CURVE('',#4418,#4419,#2488,.T.);
#5398=EDGE_CURVE('',#4419,#4419,#3847,.T.);
#5399=EDGE_CURVE('',#4356,#4420,#2489,.T.);
#5400=EDGE_CURVE('',#4420,#4421,#2490,.T.);
#5401=EDGE_CURVE('',#4357,#4421,#2491,.T.);
#5402=EDGE_CURVE('',#4422,#4341,#2492,.T.);
#5403=EDGE_CURVE('',#4423,#4422,#2493,.T.);
#5404=EDGE_CURVE('',#4423,#4339,#2494,.T.);
#5405=EDGE_CURVE('',#4376,#4423,#2495,.T.);
#5406=EDGE_CURVE('',#4377,#4422,#2496,.T.);
#5407=EDGE_CURVE('',#4424,#4361,#2497,.T.);
#5408=EDGE_CURVE('',#4425,#4424,#2498,.T.);
#5409=EDGE_CURVE('',#4425,#4359,#2499,.T.);
#5410=EDGE_CURVE('',#4396,#4425,#2500,.T.);
#5411=EDGE_CURVE('',#4397,#4424,#2501,.T.);
#5412=EDGE_CURVE('',#4426,#4381,#2502,.T.);
#5413=EDGE_CURVE('',#4427,#4426,#2503,.T.);
#5414=EDGE_CURVE('',#4427,#4379,#2504,.T.);
#5415=EDGE_CURVE('',#4416,#4427,#2505,.T.);
#5416=EDGE_CURVE('',#4417,#4426,#2506,.T.);
#5417=EDGE_CURVE('',#4421,#4401,#2507,.T.);
#5418=EDGE_CURVE('',#4420,#4399,#2508,.T.);
#5419=EDGE_CURVE('',#4428,#4429,#2509,.T.);
#5420=EDGE_CURVE('',#4430,#4428,#2510,.T.);
#5421=EDGE_CURVE('',#4431,#4430,#2511,.T.);
#5422=EDGE_CURVE('',#4429,#4431,#2512,.T.);
#5423=EDGE_CURVE('',#4430,#4432,#2513,.T.);
#5424=EDGE_CURVE('',#4433,#4432,#2514,.T.);
#5425=EDGE_CURVE('',#4431,#4433,#2515,.T.);
#5426=EDGE_CURVE('',#4432,#4434,#2516,.T.);
#5427=EDGE_CURVE('',#4434,#4435,#2517,.T.);
#5428=EDGE_CURVE('',#4435,#4433,#2518,.T.);
#5429=EDGE_CURVE('',#4436,#4436,#3848,.T.);
#5430=EDGE_CURVE('',#4437,#4428,#2519,.T.);
#5431=EDGE_CURVE('',#4438,#4437,#2520,.T.);
#5432=EDGE_CURVE('',#4438,#4439,#2521,.T.);
#5433=EDGE_CURVE('',#4440,#4439,#2522,.T.);
#5434=EDGE_CURVE('',#4440,#4441,#2523,.T.);
#5435=EDGE_CURVE('',#4441,#4442,#2524,.T.);
#5436=EDGE_CURVE('',#4442,#4434,#2525,.T.);
#5437=EDGE_CURVE('',#4442,#4443,#2526,.T.);
#5438=EDGE_CURVE('',#4443,#4435,#2527,.T.);
#5439=EDGE_CURVE('',#4444,#4441,#2528,.T.);
#5440=EDGE_CURVE('',#4443,#4444,#2529,.T.);
#5441=EDGE_CURVE('',#4445,#4444,#2530,.T.);
#5442=EDGE_CURVE('',#4446,#4445,#2531,.T.);
#5443=EDGE_CURVE('',#4446,#4447,#2532,.T.);
#5444=EDGE_CURVE('',#4448,#4447,#2533,.T.);
#5445=EDGE_CURVE('',#4448,#4429,#2534,.T.);
#5446=EDGE_CURVE('',#4445,#4440,#2535,.T.);
#5447=EDGE_CURVE('',#4439,#4449,#2536,.T.);
#5448=EDGE_CURVE('',#4449,#4450,#273,.T.);
#5449=EDGE_CURVE('',#4450,#4446,#2537,.T.);
#5450=EDGE_CURVE('',#4451,#4449,#3849,.F.);
#5451=EDGE_CURVE('',#4451,#4436,#2538,.T.);
#5452=EDGE_CURVE('',#4452,#4451,#3850,.F.);
#5453=EDGE_CURVE('',#4453,#4452,#274,.T.);
#5454=EDGE_CURVE('',#4450,#4453,#3851,.F.);
#5455=EDGE_CURVE('',#4452,#4438,#2539,.T.);
#5456=EDGE_CURVE('',#4447,#4453,#2540,.T.);
#5457=EDGE_CURVE('',#4437,#4448,#2541,.T.);
#5458=EDGE_CURVE('',#4454,#4455,#2542,.T.);
#5459=EDGE_CURVE('',#4455,#4456,#2543,.T.);
#5460=EDGE_CURVE('',#4456,#4457,#2544,.T.);
#5461=EDGE_CURVE('',#4454,#4457,#2545,.T.);
#5462=EDGE_CURVE('',#4455,#4458,#2546,.T.);
#5463=EDGE_CURVE('',#4458,#4459,#2547,.T.);
#5464=EDGE_CURVE('',#4459,#4456,#2548,.T.);
#5465=EDGE_CURVE('',#4458,#4460,#2549,.T.);
#5466=EDGE_CURVE('',#4460,#4461,#2550,.T.);
#5467=EDGE_CURVE('',#4461,#4459,#2551,.T.);
#5468=EDGE_CURVE('',#4460,#4462,#2552,.T.);
#5469=EDGE_CURVE('',#4462,#4463,#2553,.T.);
#5470=EDGE_CURVE('',#4463,#4461,#2554,.T.);
#5471=EDGE_CURVE('',#4462,#4464,#2555,.T.);
#5472=EDGE_CURVE('',#4464,#4465,#2556,.T.);
#5473=EDGE_CURVE('',#4465,#4463,#2557,.T.);
#5474=EDGE_CURVE('',#4464,#4454,#2558,.T.);
#5475=EDGE_CURVE('',#4457,#4465,#2559,.T.);
#5476=EDGE_CURVE('',#4466,#4466,#3852,.T.);
#5477=EDGE_CURVE('',#4467,#4467,#3853,.T.);
#5478=EDGE_CURVE('',#4468,#4468,#3854,.T.);
#5479=EDGE_CURVE('',#4468,#4467,#2560,.T.);
#5480=EDGE_CURVE('',#4469,#4469,#3855,.T.);
#5481=EDGE_CURVE('',#4469,#4468,#2561,.T.);
#5482=EDGE_CURVE('',#4470,#4470,#3856,.T.);
#5483=EDGE_CURVE('',#4470,#4469,#2562,.T.);
#5484=EDGE_CURVE('',#4471,#4471,#3857,.T.);
#5485=EDGE_CURVE('',#4472,#4472,#3858,.F.);
#5486=EDGE_CURVE('',#4472,#4471,#2563,.T.);
#5487=EDGE_CURVE('',#4466,#4472,#2564,.T.);
#5488=EDGE_CURVE('',#4473,#4474,#2565,.T.);
#5489=EDGE_CURVE('',#4474,#4475,#2566,.T.);
#5490=EDGE_CURVE('',#4475,#4476,#2567,.T.);
#5491=EDGE_CURVE('',#4473,#4476,#2568,.T.);
#5492=EDGE_CURVE('',#4474,#4477,#2569,.T.);
#5493=EDGE_CURVE('',#4477,#4478,#2570,.T.);
#5494=EDGE_CURVE('',#4478,#4475,#2571,.T.);
#5495=EDGE_CURVE('',#4477,#4479,#2572,.T.);
#5496=EDGE_CURVE('',#4479,#4480,#2573,.T.);
#5497=EDGE_CURVE('',#4480,#4478,#2574,.T.);
#5498=EDGE_CURVE('',#4479,#4481,#2575,.T.);
#5499=EDGE_CURVE('',#4481,#4482,#2576,.T.);
#5500=EDGE_CURVE('',#4482,#4480,#2577,.T.);
#5501=EDGE_CURVE('',#4481,#4483,#2578,.T.);
#5502=EDGE_CURVE('',#4483,#4484,#2579,.T.);
#5503=EDGE_CURVE('',#4484,#4482,#2580,.T.);
#5504=EDGE_CURVE('',#4483,#4473,#2581,.T.);
#5505=EDGE_CURVE('',#4476,#4484,#2582,.T.);
#5506=EDGE_CURVE('',#4485,#4485,#3859,.T.);
#5507=EDGE_CURVE('',#4486,#4486,#3860,.T.);
#5508=EDGE_CURVE('',#4487,#4487,#3861,.T.);
#5509=EDGE_CURVE('',#4487,#4486,#2583,.T.);
#5510=EDGE_CURVE('',#4488,#4488,#3862,.T.);
#5511=EDGE_CURVE('',#4488,#4487,#2584,.T.);
#5512=EDGE_CURVE('',#4489,#4489,#3863,.T.);
#5513=EDGE_CURVE('',#4489,#4488,#2585,.T.);
#5514=EDGE_CURVE('',#4490,#4490,#3864,.T.);
#5515=EDGE_CURVE('',#4491,#4491,#3865,.F.);
#5516=EDGE_CURVE('',#4491,#4490,#2586,.T.);
#5517=EDGE_CURVE('',#4485,#4491,#2587,.T.);
#5518=EDGE_CURVE('',#4492,#4492,#3866,.T.);
#5519=EDGE_CURVE('',#4492,#4493,#2588,.T.);
#5520=EDGE_CURVE('',#4493,#4493,#3867,.T.);
#5521=EDGE_CURVE('',#4494,#4494,#3868,.T.);
#5522=EDGE_CURVE('',#4494,#4495,#2589,.T.);
#5523=EDGE_CURVE('',#4495,#4495,#3869,.T.);
#5524=EDGE_CURVE('',#4496,#4496,#3870,.T.);
#5525=EDGE_CURVE('',#4496,#4497,#2590,.T.);
#5526=EDGE_CURVE('',#4497,#4497,#3871,.T.);
#5527=EDGE_CURVE('',#4498,#4498,#3872,.T.);
#5528=EDGE_CURVE('',#4498,#4499,#2591,.T.);
#5529=EDGE_CURVE('',#4499,#4499,#3873,.T.);
#5530=EDGE_CURVE('',#4500,#4500,#3874,.T.);
#5531=EDGE_CURVE('',#4500,#4501,#2592,.T.);
#5532=EDGE_CURVE('',#4501,#4501,#3875,.T.);
#5533=EDGE_CURVE('',#4502,#4502,#3876,.T.);
#5534=EDGE_CURVE('',#4502,#4503,#2593,.T.);
#5535=EDGE_CURVE('',#4503,#4503,#3877,.T.);
#5536=EDGE_CURVE('',#4504,#4505,#2594,.T.);
#5537=EDGE_CURVE('',#4505,#4506,#2595,.T.);
#5538=EDGE_CURVE('',#4507,#4506,#2596,.T.);
#5539=EDGE_CURVE('',#4504,#4507,#2597,.T.);
#5540=EDGE_CURVE('',#4508,#4504,#2598,.T.);
#5541=EDGE_CURVE('',#4509,#4507,#2599,.T.);
#5542=EDGE_CURVE('',#4508,#4509,#2600,.T.);
#5543=EDGE_CURVE('',#4510,#4508,#2601,.T.);
#5544=EDGE_CURVE('',#4511,#4509,#2602,.T.);
#5545=EDGE_CURVE('',#4510,#4511,#2603,.T.);
#5546=EDGE_CURVE('',#4505,#4510,#2604,.T.);
#5547=EDGE_CURVE('',#4506,#4511,#2605,.T.);
#5548=EDGE_CURVE('',#4512,#4512,#3878,.T.);
#5549=EDGE_CURVE('',#4512,#4513,#2606,.T.);
#5550=EDGE_CURVE('',#4513,#4513,#3879,.T.);
#5551=EDGE_CURVE('',#4514,#4515,#2607,.T.);
#5552=EDGE_CURVE('',#4515,#4516,#2608,.T.);
#5553=EDGE_CURVE('',#4517,#4516,#2609,.T.);
#5554=EDGE_CURVE('',#4514,#4517,#2610,.T.);
#5555=EDGE_CURVE('',#4518,#4514,#2611,.T.);
#5556=EDGE_CURVE('',#4519,#4517,#2612,.T.);
#5557=EDGE_CURVE('',#4518,#4519,#2613,.T.);
#5558=EDGE_CURVE('',#4520,#4518,#2614,.T.);
#5559=EDGE_CURVE('',#4521,#4519,#2615,.T.);
#5560=EDGE_CURVE('',#4520,#4521,#2616,.T.);
#5561=EDGE_CURVE('',#4522,#4520,#2617,.T.);
#5562=EDGE_CURVE('',#4523,#4521,#2618,.T.);
#5563=EDGE_CURVE('',#4522,#4523,#2619,.T.);
#5564=EDGE_CURVE('',#4524,#4522,#2620,.T.);
#5565=EDGE_CURVE('',#4525,#4523,#2621,.T.);
#5566=EDGE_CURVE('',#4524,#4525,#2622,.T.);
#5567=EDGE_CURVE('',#4515,#4524,#2623,.T.);
#5568=EDGE_CURVE('',#4516,#4525,#2624,.T.);
#5569=EDGE_CURVE('',#4526,#4526,#3880,.T.);
#5570=EDGE_CURVE('',#4526,#4527,#2625,.T.);
#5571=EDGE_CURVE('',#4527,#4527,#3881,.T.);
#5572=EDGE_CURVE('',#4528,#4528,#3882,.T.);
#5573=EDGE_CURVE('',#4528,#4529,#2626,.T.);
#5574=EDGE_CURVE('',#4529,#4529,#3883,.T.);
#5575=EDGE_CURVE('',#4530,#4531,#2627,.T.);
#5576=EDGE_CURVE('',#4530,#4531,#3884,.T.);
#5577=EDGE_CURVE('',#4532,#4530,#2628,.T.);
#5578=EDGE_CURVE('',#4533,#4532,#3885,.T.);
#5579=EDGE_CURVE('',#4533,#4534,#2629,.T.);
#5580=EDGE_CURVE('',#4534,#4534,#3886,.T.);
#5581=EDGE_CURVE('',#4535,#4533,#3887,.T.);
#5582=EDGE_CURVE('',#4531,#4535,#2630,.T.);
#5583=EDGE_CURVE('',#4536,#4537,#2631,.T.);
#5584=EDGE_CURVE('',#4536,#4537,#3888,.T.);
#5585=EDGE_CURVE('',#4538,#4536,#2632,.T.);
#5586=EDGE_CURVE('',#4539,#4538,#3889,.T.);
#5587=EDGE_CURVE('',#4539,#4540,#2633,.T.);
#5588=EDGE_CURVE('',#4540,#4540,#3890,.T.);
#5589=EDGE_CURVE('',#4541,#4539,#3891,.T.);
#5590=EDGE_CURVE('',#4537,#4541,#2634,.T.);
#5591=EDGE_CURVE('',#4542,#4543,#2635,.T.);
#5592=EDGE_CURVE('',#4542,#4543,#3892,.T.);
#5593=EDGE_CURVE('',#4544,#4542,#2636,.T.);
#5594=EDGE_CURVE('',#4545,#4544,#3893,.T.);
#5595=EDGE_CURVE('',#4545,#4546,#2637,.T.);
#5596=EDGE_CURVE('',#4546,#4546,#3894,.T.);
#5597=EDGE_CURVE('',#4547,#4545,#3895,.T.);
#5598=EDGE_CURVE('',#4543,#4547,#2638,.T.);
#5599=EDGE_CURVE('',#4548,#4549,#2639,.T.);
#5600=EDGE_CURVE('',#4548,#4549,#3896,.T.);
#5601=EDGE_CURVE('',#4550,#4548,#2640,.T.);
#5602=EDGE_CURVE('',#4551,#4550,#3897,.T.);
#5603=EDGE_CURVE('',#4551,#4552,#2641,.T.);
#5604=EDGE_CURVE('',#4552,#4552,#3898,.T.);
#5605=EDGE_CURVE('',#4553,#4551,#3899,.T.);
#5606=EDGE_CURVE('',#4549,#4553,#2642,.T.);
#5607=EDGE_CURVE('',#4535,#4544,#2643,.T.);
#5608=EDGE_CURVE('',#4547,#4554,#2644,.T.);
#5609=EDGE_CURVE('',#4555,#4554,#2645,.T.);
#5610=EDGE_CURVE('',#4555,#4556,#2646,.T.);
#5611=EDGE_CURVE('',#4557,#4556,#2647,.T.);
#5612=EDGE_CURVE('',#4557,#4532,#2648,.T.);
#5613=EDGE_CURVE('',#4541,#4550,#2649,.T.);
#5614=EDGE_CURVE('',#4553,#4558,#2650,.T.);
#5615=EDGE_CURVE('',#4559,#4558,#2651,.T.);
#5616=EDGE_CURVE('',#4560,#4559,#2652,.T.);
#5617=EDGE_CURVE('',#4561,#4560,#2653,.T.);
#5618=EDGE_CURVE('',#4561,#4538,#2654,.T.);
#5619=EDGE_CURVE('',#4554,#4562,#2655,.T.);
#5620=EDGE_CURVE('',#4562,#4563,#2656,.T.);
#5621=EDGE_CURVE('',#4563,#4564,#2657,.T.);
#5622=EDGE_CURVE('',#4564,#4565,#2658,.T.);
#5623=EDGE_CURVE('',#4565,#4561,#2659,.T.);
#5624=EDGE_CURVE('',#4560,#4566,#2660,.T.);
#5625=EDGE_CURVE('',#4566,#4567,#2661,.T.);
#5626=EDGE_CURVE('',#4567,#4568,#2662,.T.);
#5627=EDGE_CURVE('',#4568,#4569,#2663,.T.);
#5628=EDGE_CURVE('',#4569,#4555,#2664,.T.);
#5629=EDGE_CURVE('',#4570,#4557,#2665,.T.);
#5630=EDGE_CURVE('',#4562,#4570,#2666,.T.);
#5631=EDGE_CURVE('',#4571,#4570,#2667,.T.);
#5632=EDGE_CURVE('',#4563,#4571,#2668,.T.);
#5633=EDGE_CURVE('',#4572,#4571,#2669,.T.);
#5634=EDGE_CURVE('',#4564,#4572,#2670,.T.);
#5635=EDGE_CURVE('',#4573,#4572,#2671,.T.);
#5636=EDGE_CURVE('',#4565,#4573,#2672,.T.);
#5637=EDGE_CURVE('',#4558,#4573,#2673,.T.);
#5638=EDGE_CURVE('',#4574,#4559,#2674,.T.);
#5639=EDGE_CURVE('',#4566,#4574,#2675,.T.);
#5640=EDGE_CURVE('',#4575,#4574,#2676,.T.);
#5641=EDGE_CURVE('',#4567,#4575,#2677,.T.);
#5642=EDGE_CURVE('',#4576,#4575,#2678,.T.);
#5643=EDGE_CURVE('',#4568,#4576,#2679,.T.);
#5644=EDGE_CURVE('',#4577,#4576,#2680,.T.);
#5645=EDGE_CURVE('',#4569,#4577,#2681,.T.);
#5646=EDGE_CURVE('',#4556,#4577,#2682,.T.);
#5647=EDGE_CURVE('',#4578,#4579,#2683,.T.);
#5648=EDGE_CURVE('',#4579,#4580,#2684,.T.);
#5649=EDGE_CURVE('',#4581,#4580,#2685,.T.);
#5650=EDGE_CURVE('',#4578,#4581,#2686,.T.);
#5651=EDGE_CURVE('',#4582,#4578,#2687,.T.);
#5652=EDGE_CURVE('',#4583,#4581,#2688,.T.);
#5653=EDGE_CURVE('',#4582,#4583,#2689,.T.);
#5654=EDGE_CURVE('',#4584,#4582,#2690,.T.);
#5655=EDGE_CURVE('',#4585,#4583,#2691,.T.);
#5656=EDGE_CURVE('',#4584,#4585,#2692,.T.);
#5657=EDGE_CURVE('',#4586,#4584,#2693,.T.);
#5658=EDGE_CURVE('',#4587,#4585,#2694,.T.);
#5659=EDGE_CURVE('',#4586,#4587,#2695,.T.);
#5660=EDGE_CURVE('',#4588,#4586,#2696,.T.);
#5661=EDGE_CURVE('',#4589,#4587,#2697,.T.);
#5662=EDGE_CURVE('',#4588,#4589,#2698,.T.);
#5663=EDGE_CURVE('',#4590,#4588,#2699,.T.);
#5664=EDGE_CURVE('',#4591,#4589,#2700,.T.);
#5665=EDGE_CURVE('',#4590,#4591,#2701,.T.);
#5666=EDGE_CURVE('',#4592,#4590,#2702,.T.);
#5667=EDGE_CURVE('',#4593,#4591,#2703,.T.);
#5668=EDGE_CURVE('',#4592,#4593,#2704,.T.);
#5669=EDGE_CURVE('',#4579,#4592,#2705,.T.);
#5670=EDGE_CURVE('',#4580,#4593,#2706,.T.);
#5671=EDGE_CURVE('',#4594,#4595,#2707,.T.);
#5672=EDGE_CURVE('',#4594,#4596,#2708,.T.);
#5673=EDGE_CURVE('',#4597,#4596,#2709,.T.);
#5674=EDGE_CURVE('',#4595,#4597,#2710,.T.);
#5675=EDGE_CURVE('',#4595,#4598,#2711,.T.);
#5676=EDGE_CURVE('',#4599,#4597,#2712,.T.);
#5677=EDGE_CURVE('',#4598,#4599,#2713,.T.);
#5678=EDGE_CURVE('',#4598,#4600,#2714,.T.);
#5679=EDGE_CURVE('',#4601,#4599,#2715,.T.);
#5680=EDGE_CURVE('',#4600,#4601,#2716,.T.);
#5681=EDGE_CURVE('',#4600,#4602,#2717,.T.);
#5682=EDGE_CURVE('',#4603,#4601,#2718,.T.);
#5683=EDGE_CURVE('',#4602,#4603,#2719,.T.);
#5684=EDGE_CURVE('',#4602,#4604,#2720,.T.);
#5685=EDGE_CURVE('',#4605,#4603,#2721,.T.);
#5686=EDGE_CURVE('',#4604,#4605,#2722,.T.);
#5687=EDGE_CURVE('',#4604,#4606,#2723,.T.);
#5688=EDGE_CURVE('',#4607,#4605,#2724,.T.);
#5689=EDGE_CURVE('',#4606,#4607,#2725,.T.);
#5690=EDGE_CURVE('',#4606,#4608,#2726,.T.);
#5691=EDGE_CURVE('',#4609,#4607,#2727,.T.);
#5692=EDGE_CURVE('',#4608,#4609,#2728,.T.);
#5693=EDGE_CURVE('',#4608,#4594,#2729,.T.);
#5694=EDGE_CURVE('',#4596,#4609,#2730,.T.);
#5695=EDGE_CURVE('',#4610,#4610,#3900,.T.);
#5696=EDGE_CURVE('',#4610,#4611,#2731,.T.);
#5697=EDGE_CURVE('',#4611,#4611,#3901,.T.);
#5698=EDGE_CURVE('',#4611,#4612,#2732,.T.);
#5699=EDGE_CURVE('',#4612,#4612,#3902,.T.);
#5700=EDGE_CURVE('',#4613,#4613,#3903,.T.);
#5701=EDGE_CURVE('',#4613,#4614,#2733,.T.);
#5702=EDGE_CURVE('',#4614,#4614,#3904,.T.);
#5703=EDGE_CURVE('',#4615,#4615,#3905,.T.);
#5704=EDGE_CURVE('',#4616,#4616,#3906,.T.);
#5705=EDGE_CURVE('',#4616,#4615,#2734,.T.);
#5706=EDGE_CURVE('',#4617,#4617,#3907,.T.);
#5707=EDGE_CURVE('',#4617,#4616,#2735,.T.);
#5708=EDGE_CURVE('',#4618,#4618,#3908,.T.);
#5709=EDGE_CURVE('',#4618,#4617,#2736,.T.);
#5710=EDGE_CURVE('',#4619,#4619,#3909,.T.);
#5711=EDGE_CURVE('',#4620,#4620,#3910,.F.);
#5712=EDGE_CURVE('',#4620,#4619,#2737,.T.);
#5713=EDGE_CURVE('',#4621,#4621,#3911,.F.);
#5714=EDGE_CURVE('',#4621,#4620,#2738,.T.);
#5715=EDGE_CURVE('',#4622,#4622,#3912,.T.);
#5716=EDGE_CURVE('',#4622,#4621,#2739,.T.);
#5717=EDGE_CURVE('',#4623,#4624,#2740,.T.);
#5718=EDGE_CURVE('',#4624,#4625,#2741,.T.);
#5719=EDGE_CURVE('',#4625,#4626,#2742,.T.);
#5720=EDGE_CURVE('',#4623,#4626,#2743,.T.);
#5721=EDGE_CURVE('',#4624,#4627,#2744,.T.);
#5722=EDGE_CURVE('',#4627,#4628,#2745,.T.);
#5723=EDGE_CURVE('',#4628,#4625,#2746,.T.);
#5724=EDGE_CURVE('',#4627,#4629,#2747,.T.);
#5725=EDGE_CURVE('',#4629,#4630,#2748,.T.);
#5726=EDGE_CURVE('',#4630,#4628,#2749,.T.);
#5727=EDGE_CURVE('',#4629,#4631,#2750,.T.);
#5728=EDGE_CURVE('',#4631,#4632,#2751,.T.);
#5729=EDGE_CURVE('',#4632,#4630,#2752,.T.);
#5730=EDGE_CURVE('',#4631,#4633,#2753,.T.);
#5731=EDGE_CURVE('',#4633,#4634,#2754,.T.);
#5732=EDGE_CURVE('',#4634,#4632,#2755,.T.);
#5733=EDGE_CURVE('',#4633,#4623,#2756,.T.);
#5734=EDGE_CURVE('',#4626,#4634,#2757,.T.);
#5735=EDGE_CURVE('',#4635,#4635,#3913,.T.);
#5736=EDGE_CURVE('',#4635,#4636,#2758,.T.);
#5737=EDGE_CURVE('',#4636,#4636,#3914,.T.);
#5738=EDGE_CURVE('',#4636,#4637,#2759,.T.);
#5739=EDGE_CURVE('',#4637,#4637,#3915,.T.);
#5740=EDGE_CURVE('',#4638,#4638,#3916,.T.);
#5741=EDGE_CURVE('',#4638,#4639,#2760,.T.);
#5742=EDGE_CURVE('',#4639,#4639,#3917,.T.);
#5743=EDGE_CURVE('',#4640,#4640,#3918,.T.);
#5744=EDGE_CURVE('',#4641,#4641,#3919,.T.);
#5745=EDGE_CURVE('',#4641,#4640,#2761,.T.);
#5746=EDGE_CURVE('',#4642,#4642,#3920,.T.);
#5747=EDGE_CURVE('',#4642,#4641,#2762,.T.);
#5748=EDGE_CURVE('',#4643,#4643,#3921,.T.);
#5749=EDGE_CURVE('',#4643,#4642,#2763,.T.);
#5750=EDGE_CURVE('',#4644,#4644,#3922,.T.);
#5751=EDGE_CURVE('',#4645,#4645,#3923,.F.);
#5752=EDGE_CURVE('',#4645,#4644,#2764,.T.);
#5753=EDGE_CURVE('',#4646,#4646,#3924,.F.);
#5754=EDGE_CURVE('',#4646,#4645,#2765,.T.);
#5755=EDGE_CURVE('',#4647,#4647,#3925,.T.);
#5756=EDGE_CURVE('',#4647,#4646,#2766,.T.);
#5757=EDGE_CURVE('',#4648,#4649,#2767,.T.);
#5758=EDGE_CURVE('',#4649,#4650,#2768,.T.);
#5759=EDGE_CURVE('',#4650,#4651,#2769,.T.);
#5760=EDGE_CURVE('',#4648,#4651,#2770,.T.);
#5761=EDGE_CURVE('',#4649,#4652,#2771,.T.);
#5762=EDGE_CURVE('',#4652,#4653,#2772,.T.);
#5763=EDGE_CURVE('',#4653,#4650,#2773,.T.);
#5764=EDGE_CURVE('',#4652,#4654,#2774,.T.);
#5765=EDGE_CURVE('',#4654,#4655,#2775,.T.);
#5766=EDGE_CURVE('',#4655,#4653,#2776,.T.);
#5767=EDGE_CURVE('',#4654,#4656,#2777,.T.);
#5768=EDGE_CURVE('',#4656,#4657,#2778,.T.);
#5769=EDGE_CURVE('',#4657,#4655,#2779,.T.);
#5770=EDGE_CURVE('',#4656,#4658,#2780,.T.);
#5771=EDGE_CURVE('',#4658,#4659,#2781,.T.);
#5772=EDGE_CURVE('',#4659,#4657,#2782,.T.);
#5773=EDGE_CURVE('',#4658,#4648,#2783,.T.);
#5774=EDGE_CURVE('',#4651,#4659,#2784,.T.);
#5775=EDGE_CURVE('',#4660,#4660,#3926,.T.);
#5776=EDGE_CURVE('',#4660,#4661,#2785,.T.);
#5777=EDGE_CURVE('',#4661,#4661,#3927,.T.);
#5778=EDGE_CURVE('',#4662,#4662,#3928,.T.);
#5779=EDGE_CURVE('',#4662,#4663,#2786,.T.);
#5780=EDGE_CURVE('',#4663,#4663,#3929,.T.);
#5781=EDGE_CURVE('',#4664,#4664,#3930,.T.);
#5782=EDGE_CURVE('',#4665,#4665,#3931,.T.);
#5783=EDGE_CURVE('',#4665,#4664,#2787,.T.);
#5784=EDGE_CURVE('',#4666,#4666,#3932,.T.);
#5785=EDGE_CURVE('',#4666,#4665,#2788,.T.);
#5786=EDGE_CURVE('',#4667,#4667,#3933,.T.);
#5787=EDGE_CURVE('',#4667,#4666,#2789,.T.);
#5788=EDGE_CURVE('',#4668,#4668,#3934,.T.);
#5789=EDGE_CURVE('',#4669,#4669,#3935,.F.);
#5790=EDGE_CURVE('',#4669,#4668,#2790,.T.);
#5791=EDGE_CURVE('',#4670,#4670,#3936,.F.);
#5792=EDGE_CURVE('',#4670,#4669,#2791,.T.);
#5793=EDGE_CURVE('',#4671,#4671,#3937,.T.);
#5794=EDGE_CURVE('',#4671,#4670,#2792,.T.);
#5795=EDGE_CURVE('',#4672,#4673,#2793,.T.);
#5796=EDGE_CURVE('',#4673,#4674,#2794,.T.);
#5797=EDGE_CURVE('',#4674,#4675,#2795,.T.);
#5798=EDGE_CURVE('',#4672,#4675,#2796,.T.);
#5799=EDGE_CURVE('',#4673,#4676,#2797,.T.);
#5800=EDGE_CURVE('',#4676,#4677,#2798,.T.);
#5801=EDGE_CURVE('',#4677,#4674,#2799,.T.);
#5802=EDGE_CURVE('',#4676,#4678,#2800,.T.);
#5803=EDGE_CURVE('',#4678,#4679,#2801,.T.);
#5804=EDGE_CURVE('',#4679,#4677,#2802,.T.);
#5805=EDGE_CURVE('',#4678,#4680,#2803,.T.);
#5806=EDGE_CURVE('',#4680,#4681,#2804,.T.);
#5807=EDGE_CURVE('',#4681,#4679,#2805,.T.);
#5808=EDGE_CURVE('',#4680,#4682,#2806,.T.);
#5809=EDGE_CURVE('',#4682,#4683,#2807,.T.);
#5810=EDGE_CURVE('',#4683,#4681,#2808,.T.);
#5811=EDGE_CURVE('',#4682,#4672,#2809,.T.);
#5812=EDGE_CURVE('',#4675,#4683,#2810,.T.);
#5813=ORIENTED_EDGE('',*,*,#4684,.F.);
#5814=ORIENTED_EDGE('',*,*,#4685,.T.);
#5815=ORIENTED_EDGE('',*,*,#4686,.F.);
#5816=ORIENTED_EDGE('',*,*,#4685,.F.);
#5817=ORIENTED_EDGE('',*,*,#4687,.F.);
#5818=ORIENTED_EDGE('',*,*,#4688,.T.);
#5819=ORIENTED_EDGE('',*,*,#4689,.F.);
#5820=ORIENTED_EDGE('',*,*,#4688,.F.);
#5821=ORIENTED_EDGE('',*,*,#4690,.F.);
#5822=ORIENTED_EDGE('',*,*,#4691,.T.);
#5823=ORIENTED_EDGE('',*,*,#4692,.F.);
#5824=ORIENTED_EDGE('',*,*,#4691,.F.);
#5825=ORIENTED_EDGE('',*,*,#4693,.F.);
#5826=ORIENTED_EDGE('',*,*,#4694,.T.);
#5827=ORIENTED_EDGE('',*,*,#4695,.F.);
#5828=ORIENTED_EDGE('',*,*,#4694,.F.);
#5829=ORIENTED_EDGE('',*,*,#4696,.F.);
#5830=ORIENTED_EDGE('',*,*,#4697,.T.);
#5831=ORIENTED_EDGE('',*,*,#4698,.F.);
#5832=ORIENTED_EDGE('',*,*,#4697,.F.);
#5833=ORIENTED_EDGE('',*,*,#4699,.F.);
#5834=ORIENTED_EDGE('',*,*,#4700,.T.);
#5835=ORIENTED_EDGE('',*,*,#4701,.F.);
#5836=ORIENTED_EDGE('',*,*,#4700,.F.);
#5837=ORIENTED_EDGE('',*,*,#4702,.F.);
#5838=ORIENTED_EDGE('',*,*,#4703,.T.);
#5839=ORIENTED_EDGE('',*,*,#4704,.F.);
#5840=ORIENTED_EDGE('',*,*,#4703,.F.);
#5841=ORIENTED_EDGE('',*,*,#4705,.F.);
#5842=ORIENTED_EDGE('',*,*,#4706,.T.);
#5843=ORIENTED_EDGE('',*,*,#4707,.F.);
#5844=ORIENTED_EDGE('',*,*,#4706,.F.);
#5845=ORIENTED_EDGE('',*,*,#4708,.F.);
#5846=ORIENTED_EDGE('',*,*,#4709,.T.);
#5847=ORIENTED_EDGE('',*,*,#4710,.F.);
#5848=ORIENTED_EDGE('',*,*,#4709,.F.);
#5849=ORIENTED_EDGE('',*,*,#4711,.F.);
#5850=ORIENTED_EDGE('',*,*,#4712,.T.);
#5851=ORIENTED_EDGE('',*,*,#4713,.F.);
#5852=ORIENTED_EDGE('',*,*,#4712,.F.);
#5853=ORIENTED_EDGE('',*,*,#4714,.F.);
#5854=ORIENTED_EDGE('',*,*,#4715,.T.);
#5855=ORIENTED_EDGE('',*,*,#4716,.F.);
#5856=ORIENTED_EDGE('',*,*,#4715,.F.);
#5857=ORIENTED_EDGE('',*,*,#4717,.F.);
#5858=ORIENTED_EDGE('',*,*,#4718,.T.);
#5859=ORIENTED_EDGE('',*,*,#4719,.F.);
#5860=ORIENTED_EDGE('',*,*,#4718,.F.);
#5861=ORIENTED_EDGE('',*,*,#4720,.F.);
#5862=ORIENTED_EDGE('',*,*,#4721,.T.);
#5863=ORIENTED_EDGE('',*,*,#4722,.F.);
#5864=ORIENTED_EDGE('',*,*,#4721,.F.);
#5865=ORIENTED_EDGE('',*,*,#4723,.F.);
#5866=ORIENTED_EDGE('',*,*,#4724,.T.);
#5867=ORIENTED_EDGE('',*,*,#4725,.F.);
#5868=ORIENTED_EDGE('',*,*,#4724,.F.);
#5869=ORIENTED_EDGE('',*,*,#4726,.T.);
#5870=ORIENTED_EDGE('',*,*,#4727,.T.);
#5871=ORIENTED_EDGE('',*,*,#4728,.F.);
#5872=ORIENTED_EDGE('',*,*,#4729,.F.);
#5873=ORIENTED_EDGE('',*,*,#4730,.T.);
#5874=ORIENTED_EDGE('',*,*,#4729,.T.);
#5875=ORIENTED_EDGE('',*,*,#4731,.F.);
#5876=ORIENTED_EDGE('',*,*,#4732,.F.);
#5877=ORIENTED_EDGE('',*,*,#4733,.T.);
#5878=ORIENTED_EDGE('',*,*,#4732,.T.);
#5879=ORIENTED_EDGE('',*,*,#4734,.F.);
#5880=ORIENTED_EDGE('',*,*,#4735,.F.);
#5881=ORIENTED_EDGE('',*,*,#4736,.T.);
#5882=ORIENTED_EDGE('',*,*,#4735,.T.);
#5883=ORIENTED_EDGE('',*,*,#4737,.F.);
#5884=ORIENTED_EDGE('',*,*,#4727,.F.);
#5885=ORIENTED_EDGE('',*,*,#4737,.T.);
#5886=ORIENTED_EDGE('',*,*,#4734,.T.);
#5887=ORIENTED_EDGE('',*,*,#4731,.T.);
#5888=ORIENTED_EDGE('',*,*,#4728,.T.);
#5889=ORIENTED_EDGE('',*,*,#4692,.T.);
#5890=ORIENTED_EDGE('',*,*,#4695,.T.);
#5891=ORIENTED_EDGE('',*,*,#4698,.T.);
#5892=ORIENTED_EDGE('',*,*,#4701,.T.);
#5893=ORIENTED_EDGE('',*,*,#4725,.T.);
#5894=ORIENTED_EDGE('',*,*,#4722,.T.);
#5895=ORIENTED_EDGE('',*,*,#4719,.T.);
#5896=ORIENTED_EDGE('',*,*,#4716,.T.);
#5897=ORIENTED_EDGE('',*,*,#4713,.T.);
#5898=ORIENTED_EDGE('',*,*,#4710,.T.);
#5899=ORIENTED_EDGE('',*,*,#4707,.T.);
#5900=ORIENTED_EDGE('',*,*,#4704,.T.);
#5901=ORIENTED_EDGE('',*,*,#4689,.T.);
#5902=ORIENTED_EDGE('',*,*,#4686,.T.);
#5903=ORIENTED_EDGE('',*,*,#4736,.F.);
#5904=ORIENTED_EDGE('',*,*,#4726,.F.);
#5905=ORIENTED_EDGE('',*,*,#4730,.F.);
#5906=ORIENTED_EDGE('',*,*,#4733,.F.);
#5907=ORIENTED_EDGE('',*,*,#4690,.T.);
#5908=ORIENTED_EDGE('',*,*,#4693,.T.);
#5909=ORIENTED_EDGE('',*,*,#4696,.T.);
#5910=ORIENTED_EDGE('',*,*,#4699,.T.);
#5911=ORIENTED_EDGE('',*,*,#4723,.T.);
#5912=ORIENTED_EDGE('',*,*,#4720,.T.);
#5913=ORIENTED_EDGE('',*,*,#4717,.T.);
#5914=ORIENTED_EDGE('',*,*,#4714,.T.);
#5915=ORIENTED_EDGE('',*,*,#4711,.T.);
#5916=ORIENTED_EDGE('',*,*,#4708,.T.);
#5917=ORIENTED_EDGE('',*,*,#4705,.T.);
#5918=ORIENTED_EDGE('',*,*,#4702,.T.);
#5919=ORIENTED_EDGE('',*,*,#4687,.T.);
#5920=ORIENTED_EDGE('',*,*,#4684,.T.);
#5921=ORIENTED_EDGE('',*,*,#4738,.F.);
#5922=ORIENTED_EDGE('',*,*,#4739,.T.);
#5923=ORIENTED_EDGE('',*,*,#4740,.F.);
#5924=ORIENTED_EDGE('',*,*,#4739,.F.);
#5925=ORIENTED_EDGE('',*,*,#4738,.T.);
#5926=ORIENTED_EDGE('',*,*,#4741,.F.);
#5927=ORIENTED_EDGE('',*,*,#4742,.F.);
#5928=ORIENTED_EDGE('',*,*,#4743,.T.);
#5929=ORIENTED_EDGE('',*,*,#4744,.F.);
#5930=ORIENTED_EDGE('',*,*,#4743,.F.);
#5931=ORIENTED_EDGE('',*,*,#4742,.T.);
#5932=ORIENTED_EDGE('',*,*,#4745,.F.);
#5933=ORIENTED_EDGE('',*,*,#4746,.F.);
#5934=ORIENTED_EDGE('',*,*,#4747,.T.);
#5935=ORIENTED_EDGE('',*,*,#4741,.T.);
#5936=ORIENTED_EDGE('',*,*,#4747,.F.);
#5937=ORIENTED_EDGE('',*,*,#4748,.F.);
#5938=ORIENTED_EDGE('',*,*,#4749,.T.);
#5939=ORIENTED_EDGE('',*,*,#4745,.T.);
#5940=ORIENTED_EDGE('',*,*,#4749,.F.);
#5941=ORIENTED_EDGE('',*,*,#4750,.T.);
#5942=ORIENTED_EDGE('',*,*,#4751,.T.);
#5943=ORIENTED_EDGE('',*,*,#4752,.F.);
#5944=ORIENTED_EDGE('',*,*,#4753,.F.);
#5945=ORIENTED_EDGE('',*,*,#4754,.T.);
#5946=ORIENTED_EDGE('',*,*,#4753,.T.);
#5947=ORIENTED_EDGE('',*,*,#4755,.F.);
#5948=ORIENTED_EDGE('',*,*,#4756,.F.);
#5949=ORIENTED_EDGE('',*,*,#4757,.T.);
#5950=ORIENTED_EDGE('',*,*,#4756,.T.);
#5951=ORIENTED_EDGE('',*,*,#4758,.F.);
#5952=ORIENTED_EDGE('',*,*,#4759,.F.);
#5953=ORIENTED_EDGE('',*,*,#4760,.T.);
#5954=ORIENTED_EDGE('',*,*,#4759,.T.);
#5955=ORIENTED_EDGE('',*,*,#4761,.F.);
#5956=ORIENTED_EDGE('',*,*,#4751,.F.);
#5957=ORIENTED_EDGE('',*,*,#4761,.T.);
#5958=ORIENTED_EDGE('',*,*,#4758,.T.);
#5959=ORIENTED_EDGE('',*,*,#4755,.T.);
#5960=ORIENTED_EDGE('',*,*,#4752,.T.);
#5961=ORIENTED_EDGE('',*,*,#4740,.T.);
#5962=ORIENTED_EDGE('',*,*,#4744,.T.);
#5963=ORIENTED_EDGE('',*,*,#4760,.F.);
#5964=ORIENTED_EDGE('',*,*,#4750,.F.);
#5965=ORIENTED_EDGE('',*,*,#4754,.F.);
#5966=ORIENTED_EDGE('',*,*,#4757,.F.);
#5967=ORIENTED_EDGE('',*,*,#4746,.T.);
#5968=ORIENTED_EDGE('',*,*,#4748,.T.);
#5969=ORIENTED_EDGE('',*,*,#4762,.T.);
#5970=ORIENTED_EDGE('',*,*,#4763,.T.);
#5971=ORIENTED_EDGE('',*,*,#4764,.F.);
#5972=ORIENTED_EDGE('',*,*,#4765,.F.);
#5973=ORIENTED_EDGE('',*,*,#4766,.T.);
#5974=ORIENTED_EDGE('',*,*,#4765,.T.);
#5975=ORIENTED_EDGE('',*,*,#4767,.F.);
#5976=ORIENTED_EDGE('',*,*,#4768,.F.);
#5977=ORIENTED_EDGE('',*,*,#4769,.T.);
#5978=ORIENTED_EDGE('',*,*,#4768,.T.);
#5979=ORIENTED_EDGE('',*,*,#4770,.F.);
#5980=ORIENTED_EDGE('',*,*,#4771,.F.);
#5981=ORIENTED_EDGE('',*,*,#4772,.T.);
#5982=ORIENTED_EDGE('',*,*,#4771,.T.);
#5983=ORIENTED_EDGE('',*,*,#4773,.F.);
#5984=ORIENTED_EDGE('',*,*,#4763,.F.);
#5985=ORIENTED_EDGE('',*,*,#4773,.T.);
#5986=ORIENTED_EDGE('',*,*,#4770,.T.);
#5987=ORIENTED_EDGE('',*,*,#4767,.T.);
#5988=ORIENTED_EDGE('',*,*,#4764,.T.);
#5989=ORIENTED_EDGE('',*,*,#4772,.F.);
#5990=ORIENTED_EDGE('',*,*,#4762,.F.);
#5991=ORIENTED_EDGE('',*,*,#4766,.F.);
#5992=ORIENTED_EDGE('',*,*,#4769,.F.);
#5993=ORIENTED_EDGE('',*,*,#4774,.F.);
#5994=ORIENTED_EDGE('',*,*,#4775,.T.);
#5995=ORIENTED_EDGE('',*,*,#4776,.F.);
#5996=ORIENTED_EDGE('',*,*,#4775,.F.);
#5997=ORIENTED_EDGE('',*,*,#4774,.T.);
#5998=ORIENTED_EDGE('',*,*,#4777,.F.);
#5999=ORIENTED_EDGE('',*,*,#4778,.F.);
#6000=ORIENTED_EDGE('',*,*,#4779,.T.);
#6001=ORIENTED_EDGE('',*,*,#4780,.F.);
#6002=ORIENTED_EDGE('',*,*,#4779,.F.);
#6003=ORIENTED_EDGE('',*,*,#4778,.T.);
#6004=ORIENTED_EDGE('',*,*,#4781,.F.);
#6005=ORIENTED_EDGE('',*,*,#4782,.F.);
#6006=ORIENTED_EDGE('',*,*,#4783,.T.);
#6007=ORIENTED_EDGE('',*,*,#4777,.T.);
#6008=ORIENTED_EDGE('',*,*,#4783,.F.);
#6009=ORIENTED_EDGE('',*,*,#4784,.F.);
#6010=ORIENTED_EDGE('',*,*,#4785,.T.);
#6011=ORIENTED_EDGE('',*,*,#4781,.T.);
#6012=ORIENTED_EDGE('',*,*,#4785,.F.);
#6013=ORIENTED_EDGE('',*,*,#4786,.T.);
#6014=ORIENTED_EDGE('',*,*,#4787,.T.);
#6015=ORIENTED_EDGE('',*,*,#4788,.F.);
#6016=ORIENTED_EDGE('',*,*,#4789,.F.);
#6017=ORIENTED_EDGE('',*,*,#4790,.T.);
#6018=ORIENTED_EDGE('',*,*,#4789,.T.);
#6019=ORIENTED_EDGE('',*,*,#4791,.F.);
#6020=ORIENTED_EDGE('',*,*,#4792,.F.);
#6021=ORIENTED_EDGE('',*,*,#4793,.T.);
#6022=ORIENTED_EDGE('',*,*,#4792,.T.);
#6023=ORIENTED_EDGE('',*,*,#4794,.F.);
#6024=ORIENTED_EDGE('',*,*,#4795,.F.);
#6025=ORIENTED_EDGE('',*,*,#4796,.T.);
#6026=ORIENTED_EDGE('',*,*,#4795,.T.);
#6027=ORIENTED_EDGE('',*,*,#4797,.F.);
#6028=ORIENTED_EDGE('',*,*,#4787,.F.);
#6029=ORIENTED_EDGE('',*,*,#4797,.T.);
#6030=ORIENTED_EDGE('',*,*,#4794,.T.);
#6031=ORIENTED_EDGE('',*,*,#4791,.T.);
#6032=ORIENTED_EDGE('',*,*,#4788,.T.);
#6033=ORIENTED_EDGE('',*,*,#4776,.T.);
#6034=ORIENTED_EDGE('',*,*,#4780,.T.);
#6035=ORIENTED_EDGE('',*,*,#4796,.F.);
#6036=ORIENTED_EDGE('',*,*,#4786,.F.);
#6037=ORIENTED_EDGE('',*,*,#4790,.F.);
#6038=ORIENTED_EDGE('',*,*,#4793,.F.);
#6039=ORIENTED_EDGE('',*,*,#4782,.T.);
#6040=ORIENTED_EDGE('',*,*,#4784,.T.);
#6041=ORIENTED_EDGE('',*,*,#4798,.T.);
#6042=ORIENTED_EDGE('',*,*,#4799,.T.);
#6043=ORIENTED_EDGE('',*,*,#4800,.F.);
#6044=ORIENTED_EDGE('',*,*,#4801,.F.);
#6045=ORIENTED_EDGE('',*,*,#4802,.T.);
#6046=ORIENTED_EDGE('',*,*,#4801,.T.);
#6047=ORIENTED_EDGE('',*,*,#4803,.F.);
#6048=ORIENTED_EDGE('',*,*,#4804,.F.);
#6049=ORIENTED_EDGE('',*,*,#4805,.T.);
#6050=ORIENTED_EDGE('',*,*,#4804,.T.);
#6051=ORIENTED_EDGE('',*,*,#4806,.F.);
#6052=ORIENTED_EDGE('',*,*,#4807,.F.);
#6053=ORIENTED_EDGE('',*,*,#4808,.T.);
#6054=ORIENTED_EDGE('',*,*,#4807,.T.);
#6055=ORIENTED_EDGE('',*,*,#4809,.F.);
#6056=ORIENTED_EDGE('',*,*,#4799,.F.);
#6057=ORIENTED_EDGE('',*,*,#4809,.T.);
#6058=ORIENTED_EDGE('',*,*,#4806,.T.);
#6059=ORIENTED_EDGE('',*,*,#4803,.T.);
#6060=ORIENTED_EDGE('',*,*,#4800,.T.);
#6061=ORIENTED_EDGE('',*,*,#4808,.F.);
#6062=ORIENTED_EDGE('',*,*,#4798,.F.);
#6063=ORIENTED_EDGE('',*,*,#4802,.F.);
#6064=ORIENTED_EDGE('',*,*,#4805,.F.);
#6065=ORIENTED_EDGE('',*,*,#4810,.F.);
#6066=ORIENTED_EDGE('',*,*,#4811,.T.);
#6067=ORIENTED_EDGE('',*,*,#4812,.F.);
#6068=ORIENTED_EDGE('',*,*,#4813,.F.);
#6069=ORIENTED_EDGE('',*,*,#4814,.F.);
#6070=ORIENTED_EDGE('',*,*,#4815,.F.);
#6071=ORIENTED_EDGE('',*,*,#4816,.F.);
#6072=ORIENTED_EDGE('',*,*,#4811,.F.);
#6073=ORIENTED_EDGE('',*,*,#4817,.F.);
#6074=ORIENTED_EDGE('',*,*,#4813,.T.);
#6075=ORIENTED_EDGE('',*,*,#4818,.F.);
#6076=ORIENTED_EDGE('',*,*,#4819,.F.);
#6077=ORIENTED_EDGE('',*,*,#4817,.T.);
#6078=ORIENTED_EDGE('',*,*,#4820,.F.);
#6079=ORIENTED_EDGE('',*,*,#4814,.T.);
#6080=ORIENTED_EDGE('',*,*,#4810,.T.);
#6081=ORIENTED_EDGE('',*,*,#4821,.F.);
#6082=ORIENTED_EDGE('',*,*,#4822,.T.);
#6083=ORIENTED_EDGE('',*,*,#4823,.F.);
#6084=ORIENTED_EDGE('',*,*,#4824,.F.);
#6085=ORIENTED_EDGE('',*,*,#4825,.F.);
#6086=ORIENTED_EDGE('',*,*,#4826,.F.);
#6087=ORIENTED_EDGE('',*,*,#4827,.F.);
#6088=ORIENTED_EDGE('',*,*,#4822,.F.);
#6089=ORIENTED_EDGE('',*,*,#4828,.F.);
#6090=ORIENTED_EDGE('',*,*,#4824,.T.);
#6091=ORIENTED_EDGE('',*,*,#4829,.F.);
#6092=ORIENTED_EDGE('',*,*,#4830,.F.);
#6093=ORIENTED_EDGE('',*,*,#4828,.T.);
#6094=ORIENTED_EDGE('',*,*,#4831,.F.);
#6095=ORIENTED_EDGE('',*,*,#4825,.T.);
#6096=ORIENTED_EDGE('',*,*,#4821,.T.);
#6097=ORIENTED_EDGE('',*,*,#4832,.F.);
#6098=ORIENTED_EDGE('',*,*,#4833,.T.);
#6099=ORIENTED_EDGE('',*,*,#4834,.F.);
#6100=ORIENTED_EDGE('',*,*,#4835,.F.);
#6101=ORIENTED_EDGE('',*,*,#4836,.F.);
#6102=ORIENTED_EDGE('',*,*,#4837,.F.);
#6103=ORIENTED_EDGE('',*,*,#4838,.F.);
#6104=ORIENTED_EDGE('',*,*,#4833,.F.);
#6105=ORIENTED_EDGE('',*,*,#4839,.F.);
#6106=ORIENTED_EDGE('',*,*,#4835,.T.);
#6107=ORIENTED_EDGE('',*,*,#4840,.F.);
#6108=ORIENTED_EDGE('',*,*,#4841,.F.);
#6109=ORIENTED_EDGE('',*,*,#4839,.T.);
#6110=ORIENTED_EDGE('',*,*,#4842,.F.);
#6111=ORIENTED_EDGE('',*,*,#4836,.T.);
#6112=ORIENTED_EDGE('',*,*,#4832,.T.);
#6113=ORIENTED_EDGE('',*,*,#4843,.F.);
#6114=ORIENTED_EDGE('',*,*,#4844,.T.);
#6115=ORIENTED_EDGE('',*,*,#4845,.F.);
#6116=ORIENTED_EDGE('',*,*,#4846,.F.);
#6117=ORIENTED_EDGE('',*,*,#4847,.F.);
#6118=ORIENTED_EDGE('',*,*,#4848,.F.);
#6119=ORIENTED_EDGE('',*,*,#4849,.F.);
#6120=ORIENTED_EDGE('',*,*,#4844,.F.);
#6121=ORIENTED_EDGE('',*,*,#4850,.F.);
#6122=ORIENTED_EDGE('',*,*,#4846,.T.);
#6123=ORIENTED_EDGE('',*,*,#4851,.F.);
#6124=ORIENTED_EDGE('',*,*,#4852,.F.);
#6125=ORIENTED_EDGE('',*,*,#4850,.T.);
#6126=ORIENTED_EDGE('',*,*,#4853,.F.);
#6127=ORIENTED_EDGE('',*,*,#4847,.T.);
#6128=ORIENTED_EDGE('',*,*,#4843,.T.);
#6129=ORIENTED_EDGE('',*,*,#4854,.F.);
#6130=ORIENTED_EDGE('',*,*,#4855,.T.);
#6131=ORIENTED_EDGE('',*,*,#4856,.F.);
#6132=ORIENTED_EDGE('',*,*,#4857,.F.);
#6133=ORIENTED_EDGE('',*,*,#4858,.F.);
#6134=ORIENTED_EDGE('',*,*,#4859,.F.);
#6135=ORIENTED_EDGE('',*,*,#4860,.F.);
#6136=ORIENTED_EDGE('',*,*,#4855,.F.);
#6137=ORIENTED_EDGE('',*,*,#4861,.F.);
#6138=ORIENTED_EDGE('',*,*,#4857,.T.);
#6139=ORIENTED_EDGE('',*,*,#4862,.F.);
#6140=ORIENTED_EDGE('',*,*,#4863,.F.);
#6141=ORIENTED_EDGE('',*,*,#4861,.T.);
#6142=ORIENTED_EDGE('',*,*,#4864,.F.);
#6143=ORIENTED_EDGE('',*,*,#4858,.T.);
#6144=ORIENTED_EDGE('',*,*,#4854,.T.);
#6145=ORIENTED_EDGE('',*,*,#4865,.F.);
#6146=ORIENTED_EDGE('',*,*,#4866,.T.);
#6147=ORIENTED_EDGE('',*,*,#4867,.F.);
#6148=ORIENTED_EDGE('',*,*,#4868,.F.);
#6149=ORIENTED_EDGE('',*,*,#4869,.F.);
#6150=ORIENTED_EDGE('',*,*,#4870,.F.);
#6151=ORIENTED_EDGE('',*,*,#4871,.F.);
#6152=ORIENTED_EDGE('',*,*,#4866,.F.);
#6153=ORIENTED_EDGE('',*,*,#4872,.F.);
#6154=ORIENTED_EDGE('',*,*,#4868,.T.);
#6155=ORIENTED_EDGE('',*,*,#4873,.F.);
#6156=ORIENTED_EDGE('',*,*,#4874,.F.);
#6157=ORIENTED_EDGE('',*,*,#4872,.T.);
#6158=ORIENTED_EDGE('',*,*,#4875,.F.);
#6159=ORIENTED_EDGE('',*,*,#4869,.T.);
#6160=ORIENTED_EDGE('',*,*,#4865,.T.);
#6161=ORIENTED_EDGE('',*,*,#4876,.F.);
#6162=ORIENTED_EDGE('',*,*,#4877,.T.);
#6163=ORIENTED_EDGE('',*,*,#4878,.F.);
#6164=ORIENTED_EDGE('',*,*,#4879,.F.);
#6165=ORIENTED_EDGE('',*,*,#4880,.F.);
#6166=ORIENTED_EDGE('',*,*,#4881,.F.);
#6167=ORIENTED_EDGE('',*,*,#4882,.F.);
#6168=ORIENTED_EDGE('',*,*,#4877,.F.);
#6169=ORIENTED_EDGE('',*,*,#4883,.F.);
#6170=ORIENTED_EDGE('',*,*,#4879,.T.);
#6171=ORIENTED_EDGE('',*,*,#4884,.F.);
#6172=ORIENTED_EDGE('',*,*,#4885,.F.);
#6173=ORIENTED_EDGE('',*,*,#4883,.T.);
#6174=ORIENTED_EDGE('',*,*,#4886,.F.);
#6175=ORIENTED_EDGE('',*,*,#4880,.T.);
#6176=ORIENTED_EDGE('',*,*,#4876,.T.);
#6177=ORIENTED_EDGE('',*,*,#4887,.F.);
#6178=ORIENTED_EDGE('',*,*,#4888,.T.);
#6179=ORIENTED_EDGE('',*,*,#4889,.F.);
#6180=ORIENTED_EDGE('',*,*,#4890,.F.);
#6181=ORIENTED_EDGE('',*,*,#4891,.F.);
#6182=ORIENTED_EDGE('',*,*,#4892,.F.);
#6183=ORIENTED_EDGE('',*,*,#4893,.F.);
#6184=ORIENTED_EDGE('',*,*,#4888,.F.);
#6185=ORIENTED_EDGE('',*,*,#4894,.F.);
#6186=ORIENTED_EDGE('',*,*,#4890,.T.);
#6187=ORIENTED_EDGE('',*,*,#4895,.F.);
#6188=ORIENTED_EDGE('',*,*,#4896,.F.);
#6189=ORIENTED_EDGE('',*,*,#4894,.T.);
#6190=ORIENTED_EDGE('',*,*,#4897,.F.);
#6191=ORIENTED_EDGE('',*,*,#4891,.T.);
#6192=ORIENTED_EDGE('',*,*,#4887,.T.);
#6193=ORIENTED_EDGE('',*,*,#4898,.F.);
#6194=ORIENTED_EDGE('',*,*,#4899,.T.);
#6195=ORIENTED_EDGE('',*,*,#4900,.F.);
#6196=ORIENTED_EDGE('',*,*,#4901,.F.);
#6197=ORIENTED_EDGE('',*,*,#4902,.F.);
#6198=ORIENTED_EDGE('',*,*,#4903,.F.);
#6199=ORIENTED_EDGE('',*,*,#4904,.F.);
#6200=ORIENTED_EDGE('',*,*,#4899,.F.);
#6201=ORIENTED_EDGE('',*,*,#4905,.F.);
#6202=ORIENTED_EDGE('',*,*,#4901,.T.);
#6203=ORIENTED_EDGE('',*,*,#4906,.F.);
#6204=ORIENTED_EDGE('',*,*,#4907,.F.);
#6205=ORIENTED_EDGE('',*,*,#4905,.T.);
#6206=ORIENTED_EDGE('',*,*,#4908,.F.);
#6207=ORIENTED_EDGE('',*,*,#4902,.T.);
#6208=ORIENTED_EDGE('',*,*,#4898,.T.);
#6209=ORIENTED_EDGE('',*,*,#4909,.F.);
#6210=ORIENTED_EDGE('',*,*,#4910,.T.);
#6211=ORIENTED_EDGE('',*,*,#4911,.F.);
#6212=ORIENTED_EDGE('',*,*,#4912,.F.);
#6213=ORIENTED_EDGE('',*,*,#4913,.F.);
#6214=ORIENTED_EDGE('',*,*,#4914,.F.);
#6215=ORIENTED_EDGE('',*,*,#4915,.F.);
#6216=ORIENTED_EDGE('',*,*,#4910,.F.);
#6217=ORIENTED_EDGE('',*,*,#4916,.F.);
#6218=ORIENTED_EDGE('',*,*,#4912,.T.);
#6219=ORIENTED_EDGE('',*,*,#4917,.F.);
#6220=ORIENTED_EDGE('',*,*,#4918,.F.);
#6221=ORIENTED_EDGE('',*,*,#4916,.T.);
#6222=ORIENTED_EDGE('',*,*,#4919,.F.);
#6223=ORIENTED_EDGE('',*,*,#4913,.T.);
#6224=ORIENTED_EDGE('',*,*,#4909,.T.);
#6225=ORIENTED_EDGE('',*,*,#4920,.F.);
#6226=ORIENTED_EDGE('',*,*,#4921,.T.);
#6227=ORIENTED_EDGE('',*,*,#4922,.F.);
#6228=ORIENTED_EDGE('',*,*,#4923,.F.);
#6229=ORIENTED_EDGE('',*,*,#4924,.F.);
#6230=ORIENTED_EDGE('',*,*,#4925,.F.);
#6231=ORIENTED_EDGE('',*,*,#4926,.F.);
#6232=ORIENTED_EDGE('',*,*,#4921,.F.);
#6233=ORIENTED_EDGE('',*,*,#4927,.F.);
#6234=ORIENTED_EDGE('',*,*,#4923,.T.);
#6235=ORIENTED_EDGE('',*,*,#4928,.F.);
#6236=ORIENTED_EDGE('',*,*,#4929,.F.);
#6237=ORIENTED_EDGE('',*,*,#4927,.T.);
#6238=ORIENTED_EDGE('',*,*,#4930,.F.);
#6239=ORIENTED_EDGE('',*,*,#4924,.T.);
#6240=ORIENTED_EDGE('',*,*,#4920,.T.);
#6241=ORIENTED_EDGE('',*,*,#4931,.F.);
#6242=ORIENTED_EDGE('',*,*,#4932,.T.);
#6243=ORIENTED_EDGE('',*,*,#4933,.F.);
#6244=ORIENTED_EDGE('',*,*,#4934,.F.);
#6245=ORIENTED_EDGE('',*,*,#4935,.F.);
#6246=ORIENTED_EDGE('',*,*,#4936,.F.);
#6247=ORIENTED_EDGE('',*,*,#4937,.F.);
#6248=ORIENTED_EDGE('',*,*,#4932,.F.);
#6249=ORIENTED_EDGE('',*,*,#4938,.F.);
#6250=ORIENTED_EDGE('',*,*,#4934,.T.);
#6251=ORIENTED_EDGE('',*,*,#4939,.F.);
#6252=ORIENTED_EDGE('',*,*,#4940,.F.);
#6253=ORIENTED_EDGE('',*,*,#4938,.T.);
#6254=ORIENTED_EDGE('',*,*,#4941,.F.);
#6255=ORIENTED_EDGE('',*,*,#4935,.T.);
#6256=ORIENTED_EDGE('',*,*,#4931,.T.);
#6257=ORIENTED_EDGE('',*,*,#4942,.F.);
#6258=ORIENTED_EDGE('',*,*,#4943,.T.);
#6259=ORIENTED_EDGE('',*,*,#4944,.F.);
#6260=ORIENTED_EDGE('',*,*,#4945,.F.);
#6261=ORIENTED_EDGE('',*,*,#4946,.F.);
#6262=ORIENTED_EDGE('',*,*,#4947,.F.);
#6263=ORIENTED_EDGE('',*,*,#4948,.F.);
#6264=ORIENTED_EDGE('',*,*,#4943,.F.);
#6265=ORIENTED_EDGE('',*,*,#4949,.F.);
#6266=ORIENTED_EDGE('',*,*,#4945,.T.);
#6267=ORIENTED_EDGE('',*,*,#4950,.F.);
#6268=ORIENTED_EDGE('',*,*,#4951,.F.);
#6269=ORIENTED_EDGE('',*,*,#4949,.T.);
#6270=ORIENTED_EDGE('',*,*,#4952,.F.);
#6271=ORIENTED_EDGE('',*,*,#4946,.T.);
#6272=ORIENTED_EDGE('',*,*,#4942,.T.);
#6273=ORIENTED_EDGE('',*,*,#4953,.F.);
#6274=ORIENTED_EDGE('',*,*,#4954,.T.);
#6275=ORIENTED_EDGE('',*,*,#4955,.F.);
#6276=ORIENTED_EDGE('',*,*,#4956,.F.);
#6277=ORIENTED_EDGE('',*,*,#4957,.F.);
#6278=ORIENTED_EDGE('',*,*,#4958,.F.);
#6279=ORIENTED_EDGE('',*,*,#4959,.F.);
#6280=ORIENTED_EDGE('',*,*,#4954,.F.);
#6281=ORIENTED_EDGE('',*,*,#4960,.F.);
#6282=ORIENTED_EDGE('',*,*,#4956,.T.);
#6283=ORIENTED_EDGE('',*,*,#4961,.F.);
#6284=ORIENTED_EDGE('',*,*,#4962,.F.);
#6285=ORIENTED_EDGE('',*,*,#4960,.T.);
#6286=ORIENTED_EDGE('',*,*,#4963,.F.);
#6287=ORIENTED_EDGE('',*,*,#4957,.T.);
#6288=ORIENTED_EDGE('',*,*,#4953,.T.);
#6289=ORIENTED_EDGE('',*,*,#4964,.F.);
#6290=ORIENTED_EDGE('',*,*,#4965,.T.);
#6291=ORIENTED_EDGE('',*,*,#4966,.F.);
#6292=ORIENTED_EDGE('',*,*,#4967,.F.);
#6293=ORIENTED_EDGE('',*,*,#4968,.F.);
#6294=ORIENTED_EDGE('',*,*,#4969,.F.);
#6295=ORIENTED_EDGE('',*,*,#4970,.F.);
#6296=ORIENTED_EDGE('',*,*,#4965,.F.);
#6297=ORIENTED_EDGE('',*,*,#4971,.F.);
#6298=ORIENTED_EDGE('',*,*,#4967,.T.);
#6299=ORIENTED_EDGE('',*,*,#4972,.F.);
#6300=ORIENTED_EDGE('',*,*,#4973,.F.);
#6301=ORIENTED_EDGE('',*,*,#4971,.T.);
#6302=ORIENTED_EDGE('',*,*,#4974,.F.);
#6303=ORIENTED_EDGE('',*,*,#4968,.T.);
#6304=ORIENTED_EDGE('',*,*,#4964,.T.);
#6305=ORIENTED_EDGE('',*,*,#4975,.F.);
#6306=ORIENTED_EDGE('',*,*,#4976,.T.);
#6307=ORIENTED_EDGE('',*,*,#4977,.F.);
#6308=ORIENTED_EDGE('',*,*,#4978,.F.);
#6309=ORIENTED_EDGE('',*,*,#4979,.F.);
#6310=ORIENTED_EDGE('',*,*,#4980,.F.);
#6311=ORIENTED_EDGE('',*,*,#4981,.F.);
#6312=ORIENTED_EDGE('',*,*,#4976,.F.);
#6313=ORIENTED_EDGE('',*,*,#4982,.F.);
#6314=ORIENTED_EDGE('',*,*,#4978,.T.);
#6315=ORIENTED_EDGE('',*,*,#4983,.F.);
#6316=ORIENTED_EDGE('',*,*,#4984,.F.);
#6317=ORIENTED_EDGE('',*,*,#4982,.T.);
#6318=ORIENTED_EDGE('',*,*,#4985,.F.);
#6319=ORIENTED_EDGE('',*,*,#4979,.T.);
#6320=ORIENTED_EDGE('',*,*,#4975,.T.);
#6321=ORIENTED_EDGE('',*,*,#4986,.F.);
#6322=ORIENTED_EDGE('',*,*,#4987,.T.);
#6323=ORIENTED_EDGE('',*,*,#4988,.F.);
#6324=ORIENTED_EDGE('',*,*,#4989,.F.);
#6325=ORIENTED_EDGE('',*,*,#4990,.F.);
#6326=ORIENTED_EDGE('',*,*,#4991,.F.);
#6327=ORIENTED_EDGE('',*,*,#4992,.F.);
#6328=ORIENTED_EDGE('',*,*,#4987,.F.);
#6329=ORIENTED_EDGE('',*,*,#4993,.F.);
#6330=ORIENTED_EDGE('',*,*,#4989,.T.);
#6331=ORIENTED_EDGE('',*,*,#4994,.F.);
#6332=ORIENTED_EDGE('',*,*,#4995,.F.);
#6333=ORIENTED_EDGE('',*,*,#4993,.T.);
#6334=ORIENTED_EDGE('',*,*,#4996,.F.);
#6335=ORIENTED_EDGE('',*,*,#4990,.T.);
#6336=ORIENTED_EDGE('',*,*,#4986,.T.);
#6337=ORIENTED_EDGE('',*,*,#4997,.F.);
#6338=ORIENTED_EDGE('',*,*,#4998,.T.);
#6339=ORIENTED_EDGE('',*,*,#4999,.F.);
#6340=ORIENTED_EDGE('',*,*,#5000,.F.);
#6341=ORIENTED_EDGE('',*,*,#5001,.F.);
#6342=ORIENTED_EDGE('',*,*,#5002,.F.);
#6343=ORIENTED_EDGE('',*,*,#5003,.F.);
#6344=ORIENTED_EDGE('',*,*,#4998,.F.);
#6345=ORIENTED_EDGE('',*,*,#5004,.F.);
#6346=ORIENTED_EDGE('',*,*,#5000,.T.);
#6347=ORIENTED_EDGE('',*,*,#5005,.F.);
#6348=ORIENTED_EDGE('',*,*,#5006,.F.);
#6349=ORIENTED_EDGE('',*,*,#5004,.T.);
#6350=ORIENTED_EDGE('',*,*,#5007,.F.);
#6351=ORIENTED_EDGE('',*,*,#5001,.T.);
#6352=ORIENTED_EDGE('',*,*,#4997,.T.);
#6353=ORIENTED_EDGE('',*,*,#5008,.F.);
#6354=ORIENTED_EDGE('',*,*,#5009,.T.);
#6355=ORIENTED_EDGE('',*,*,#5010,.F.);
#6356=ORIENTED_EDGE('',*,*,#5011,.F.);
#6357=ORIENTED_EDGE('',*,*,#5012,.F.);
#6358=ORIENTED_EDGE('',*,*,#5013,.F.);
#6359=ORIENTED_EDGE('',*,*,#5014,.F.);
#6360=ORIENTED_EDGE('',*,*,#5009,.F.);
#6361=ORIENTED_EDGE('',*,*,#5015,.F.);
#6362=ORIENTED_EDGE('',*,*,#5011,.T.);
#6363=ORIENTED_EDGE('',*,*,#5016,.F.);
#6364=ORIENTED_EDGE('',*,*,#5017,.F.);
#6365=ORIENTED_EDGE('',*,*,#5015,.T.);
#6366=ORIENTED_EDGE('',*,*,#5018,.F.);
#6367=ORIENTED_EDGE('',*,*,#5012,.T.);
#6368=ORIENTED_EDGE('',*,*,#5008,.T.);
#6369=ORIENTED_EDGE('',*,*,#5019,.F.);
#6370=ORIENTED_EDGE('',*,*,#5020,.T.);
#6371=ORIENTED_EDGE('',*,*,#5021,.F.);
#6372=ORIENTED_EDGE('',*,*,#5022,.F.);
#6373=ORIENTED_EDGE('',*,*,#5023,.F.);
#6374=ORIENTED_EDGE('',*,*,#5024,.F.);
#6375=ORIENTED_EDGE('',*,*,#5025,.F.);
#6376=ORIENTED_EDGE('',*,*,#5020,.F.);
#6377=ORIENTED_EDGE('',*,*,#5026,.F.);
#6378=ORIENTED_EDGE('',*,*,#5022,.T.);
#6379=ORIENTED_EDGE('',*,*,#5027,.F.);
#6380=ORIENTED_EDGE('',*,*,#5028,.F.);
#6381=ORIENTED_EDGE('',*,*,#5026,.T.);
#6382=ORIENTED_EDGE('',*,*,#5029,.F.);
#6383=ORIENTED_EDGE('',*,*,#5023,.T.);
#6384=ORIENTED_EDGE('',*,*,#5019,.T.);
#6385=ORIENTED_EDGE('',*,*,#5030,.F.);
#6386=ORIENTED_EDGE('',*,*,#5031,.T.);
#6387=ORIENTED_EDGE('',*,*,#5032,.F.);
#6388=ORIENTED_EDGE('',*,*,#5033,.F.);
#6389=ORIENTED_EDGE('',*,*,#5034,.F.);
#6390=ORIENTED_EDGE('',*,*,#5035,.F.);
#6391=ORIENTED_EDGE('',*,*,#5036,.F.);
#6392=ORIENTED_EDGE('',*,*,#5031,.F.);
#6393=ORIENTED_EDGE('',*,*,#5037,.F.);
#6394=ORIENTED_EDGE('',*,*,#5033,.T.);
#6395=ORIENTED_EDGE('',*,*,#5038,.F.);
#6396=ORIENTED_EDGE('',*,*,#5039,.F.);
#6397=ORIENTED_EDGE('',*,*,#5037,.T.);
#6398=ORIENTED_EDGE('',*,*,#5040,.F.);
#6399=ORIENTED_EDGE('',*,*,#5034,.T.);
#6400=ORIENTED_EDGE('',*,*,#5030,.T.);
#6401=ORIENTED_EDGE('',*,*,#5041,.F.);
#6402=ORIENTED_EDGE('',*,*,#5042,.T.);
#6403=ORIENTED_EDGE('',*,*,#5043,.F.);
#6404=ORIENTED_EDGE('',*,*,#5044,.F.);
#6405=ORIENTED_EDGE('',*,*,#5045,.F.);
#6406=ORIENTED_EDGE('',*,*,#5046,.F.);
#6407=ORIENTED_EDGE('',*,*,#5047,.F.);
#6408=ORIENTED_EDGE('',*,*,#5042,.F.);
#6409=ORIENTED_EDGE('',*,*,#5048,.F.);
#6410=ORIENTED_EDGE('',*,*,#5044,.T.);
#6411=ORIENTED_EDGE('',*,*,#5049,.F.);
#6412=ORIENTED_EDGE('',*,*,#5050,.F.);
#6413=ORIENTED_EDGE('',*,*,#5048,.T.);
#6414=ORIENTED_EDGE('',*,*,#5051,.F.);
#6415=ORIENTED_EDGE('',*,*,#5045,.T.);
#6416=ORIENTED_EDGE('',*,*,#5041,.T.);
#6417=ORIENTED_EDGE('',*,*,#5052,.F.);
#6418=ORIENTED_EDGE('',*,*,#5053,.T.);
#6419=ORIENTED_EDGE('',*,*,#5054,.F.);
#6420=ORIENTED_EDGE('',*,*,#5055,.F.);
#6421=ORIENTED_EDGE('',*,*,#5056,.F.);
#6422=ORIENTED_EDGE('',*,*,#5057,.F.);
#6423=ORIENTED_EDGE('',*,*,#5058,.F.);
#6424=ORIENTED_EDGE('',*,*,#5053,.F.);
#6425=ORIENTED_EDGE('',*,*,#5059,.F.);
#6426=ORIENTED_EDGE('',*,*,#5055,.T.);
#6427=ORIENTED_EDGE('',*,*,#5060,.F.);
#6428=ORIENTED_EDGE('',*,*,#5061,.F.);
#6429=ORIENTED_EDGE('',*,*,#5059,.T.);
#6430=ORIENTED_EDGE('',*,*,#5062,.F.);
#6431=ORIENTED_EDGE('',*,*,#5056,.T.);
#6432=ORIENTED_EDGE('',*,*,#5052,.T.);
#6433=ORIENTED_EDGE('',*,*,#5063,.F.);
#6434=ORIENTED_EDGE('',*,*,#5064,.T.);
#6435=ORIENTED_EDGE('',*,*,#5065,.F.);
#6436=ORIENTED_EDGE('',*,*,#5066,.F.);
#6437=ORIENTED_EDGE('',*,*,#5067,.F.);
#6438=ORIENTED_EDGE('',*,*,#5068,.F.);
#6439=ORIENTED_EDGE('',*,*,#5069,.F.);
#6440=ORIENTED_EDGE('',*,*,#5064,.F.);
#6441=ORIENTED_EDGE('',*,*,#5070,.F.);
#6442=ORIENTED_EDGE('',*,*,#5066,.T.);
#6443=ORIENTED_EDGE('',*,*,#5071,.F.);
#6444=ORIENTED_EDGE('',*,*,#5072,.F.);
#6445=ORIENTED_EDGE('',*,*,#5070,.T.);
#6446=ORIENTED_EDGE('',*,*,#5073,.F.);
#6447=ORIENTED_EDGE('',*,*,#5067,.T.);
#6448=ORIENTED_EDGE('',*,*,#5063,.T.);
#6449=ORIENTED_EDGE('',*,*,#5074,.F.);
#6450=ORIENTED_EDGE('',*,*,#5075,.T.);
#6451=ORIENTED_EDGE('',*,*,#5076,.F.);
#6452=ORIENTED_EDGE('',*,*,#5077,.F.);
#6453=ORIENTED_EDGE('',*,*,#5078,.F.);
#6454=ORIENTED_EDGE('',*,*,#5079,.F.);
#6455=ORIENTED_EDGE('',*,*,#5080,.F.);
#6456=ORIENTED_EDGE('',*,*,#5075,.F.);
#6457=ORIENTED_EDGE('',*,*,#5081,.F.);
#6458=ORIENTED_EDGE('',*,*,#5077,.T.);
#6459=ORIENTED_EDGE('',*,*,#5082,.F.);
#6460=ORIENTED_EDGE('',*,*,#5083,.F.);
#6461=ORIENTED_EDGE('',*,*,#5081,.T.);
#6462=ORIENTED_EDGE('',*,*,#5084,.F.);
#6463=ORIENTED_EDGE('',*,*,#5078,.T.);
#6464=ORIENTED_EDGE('',*,*,#5074,.T.);
#6465=ORIENTED_EDGE('',*,*,#5085,.F.);
#6466=ORIENTED_EDGE('',*,*,#5086,.T.);
#6467=ORIENTED_EDGE('',*,*,#5087,.F.);
#6468=ORIENTED_EDGE('',*,*,#5088,.F.);
#6469=ORIENTED_EDGE('',*,*,#5089,.F.);
#6470=ORIENTED_EDGE('',*,*,#5090,.F.);
#6471=ORIENTED_EDGE('',*,*,#5091,.F.);
#6472=ORIENTED_EDGE('',*,*,#5086,.F.);
#6473=ORIENTED_EDGE('',*,*,#5092,.F.);
#6474=ORIENTED_EDGE('',*,*,#5088,.T.);
#6475=ORIENTED_EDGE('',*,*,#5093,.F.);
#6476=ORIENTED_EDGE('',*,*,#5094,.F.);
#6477=ORIENTED_EDGE('',*,*,#5092,.T.);
#6478=ORIENTED_EDGE('',*,*,#5095,.F.);
#6479=ORIENTED_EDGE('',*,*,#5089,.T.);
#6480=ORIENTED_EDGE('',*,*,#5085,.T.);
#6481=ORIENTED_EDGE('',*,*,#5096,.F.);
#6482=ORIENTED_EDGE('',*,*,#5097,.T.);
#6483=ORIENTED_EDGE('',*,*,#5098,.F.);
#6484=ORIENTED_EDGE('',*,*,#5099,.F.);
#6485=ORIENTED_EDGE('',*,*,#5100,.F.);
#6486=ORIENTED_EDGE('',*,*,#5101,.F.);
#6487=ORIENTED_EDGE('',*,*,#5102,.F.);
#6488=ORIENTED_EDGE('',*,*,#5097,.F.);
#6489=ORIENTED_EDGE('',*,*,#5103,.F.);
#6490=ORIENTED_EDGE('',*,*,#5099,.T.);
#6491=ORIENTED_EDGE('',*,*,#5104,.F.);
#6492=ORIENTED_EDGE('',*,*,#5105,.F.);
#6493=ORIENTED_EDGE('',*,*,#5103,.T.);
#6494=ORIENTED_EDGE('',*,*,#5106,.F.);
#6495=ORIENTED_EDGE('',*,*,#5100,.T.);
#6496=ORIENTED_EDGE('',*,*,#5096,.T.);
#6497=ORIENTED_EDGE('',*,*,#5107,.F.);
#6498=ORIENTED_EDGE('',*,*,#5108,.T.);
#6499=ORIENTED_EDGE('',*,*,#5109,.F.);
#6500=ORIENTED_EDGE('',*,*,#5110,.F.);
#6501=ORIENTED_EDGE('',*,*,#5111,.F.);
#6502=ORIENTED_EDGE('',*,*,#5112,.F.);
#6503=ORIENTED_EDGE('',*,*,#5113,.F.);
#6504=ORIENTED_EDGE('',*,*,#5108,.F.);
#6505=ORIENTED_EDGE('',*,*,#5114,.F.);
#6506=ORIENTED_EDGE('',*,*,#5110,.T.);
#6507=ORIENTED_EDGE('',*,*,#5115,.F.);
#6508=ORIENTED_EDGE('',*,*,#5116,.F.);
#6509=ORIENTED_EDGE('',*,*,#5114,.T.);
#6510=ORIENTED_EDGE('',*,*,#5117,.F.);
#6511=ORIENTED_EDGE('',*,*,#5111,.T.);
#6512=ORIENTED_EDGE('',*,*,#5107,.T.);
#6513=ORIENTED_EDGE('',*,*,#5118,.F.);
#6514=ORIENTED_EDGE('',*,*,#5119,.T.);
#6515=ORIENTED_EDGE('',*,*,#5120,.F.);
#6516=ORIENTED_EDGE('',*,*,#5121,.F.);
#6517=ORIENTED_EDGE('',*,*,#5122,.F.);
#6518=ORIENTED_EDGE('',*,*,#5123,.F.);
#6519=ORIENTED_EDGE('',*,*,#5124,.F.);
#6520=ORIENTED_EDGE('',*,*,#5119,.F.);
#6521=ORIENTED_EDGE('',*,*,#5125,.F.);
#6522=ORIENTED_EDGE('',*,*,#5121,.T.);
#6523=ORIENTED_EDGE('',*,*,#5126,.F.);
#6524=ORIENTED_EDGE('',*,*,#5127,.F.);
#6525=ORIENTED_EDGE('',*,*,#5125,.T.);
#6526=ORIENTED_EDGE('',*,*,#5128,.F.);
#6527=ORIENTED_EDGE('',*,*,#5122,.T.);
#6528=ORIENTED_EDGE('',*,*,#5118,.T.);
#6529=ORIENTED_EDGE('',*,*,#4818,.T.);
#6530=ORIENTED_EDGE('',*,*,#4812,.T.);
#6531=ORIENTED_EDGE('',*,*,#4816,.T.);
#6532=ORIENTED_EDGE('',*,*,#5129,.T.);
#6533=ORIENTED_EDGE('',*,*,#5126,.T.);
#6534=ORIENTED_EDGE('',*,*,#5120,.T.);
#6535=ORIENTED_EDGE('',*,*,#5124,.T.);
#6536=ORIENTED_EDGE('',*,*,#5130,.T.);
#6537=ORIENTED_EDGE('',*,*,#5131,.T.);
#6538=ORIENTED_EDGE('',*,*,#5132,.T.);
#6539=ORIENTED_EDGE('',*,*,#5133,.T.);
#6540=ORIENTED_EDGE('',*,*,#5134,.T.);
#6541=ORIENTED_EDGE('',*,*,#5049,.T.);
#6542=ORIENTED_EDGE('',*,*,#5043,.T.);
#6543=ORIENTED_EDGE('',*,*,#5047,.T.);
#6544=ORIENTED_EDGE('',*,*,#5135,.T.);
#6545=ORIENTED_EDGE('',*,*,#4972,.T.);
#6546=ORIENTED_EDGE('',*,*,#4966,.T.);
#6547=ORIENTED_EDGE('',*,*,#4970,.T.);
#6548=ORIENTED_EDGE('',*,*,#5136,.T.);
#6549=ORIENTED_EDGE('',*,*,#4961,.T.);
#6550=ORIENTED_EDGE('',*,*,#4955,.T.);
#6551=ORIENTED_EDGE('',*,*,#4959,.T.);
#6552=ORIENTED_EDGE('',*,*,#5137,.T.);
#6553=ORIENTED_EDGE('',*,*,#4983,.T.);
#6554=ORIENTED_EDGE('',*,*,#4977,.T.);
#6555=ORIENTED_EDGE('',*,*,#4981,.T.);
#6556=ORIENTED_EDGE('',*,*,#5138,.T.);
#6557=ORIENTED_EDGE('',*,*,#4950,.T.);
#6558=ORIENTED_EDGE('',*,*,#4944,.T.);
#6559=ORIENTED_EDGE('',*,*,#4948,.T.);
#6560=ORIENTED_EDGE('',*,*,#5139,.T.);
#6561=ORIENTED_EDGE('',*,*,#4994,.T.);
#6562=ORIENTED_EDGE('',*,*,#4988,.T.);
#6563=ORIENTED_EDGE('',*,*,#4992,.T.);
#6564=ORIENTED_EDGE('',*,*,#5140,.T.);
#6565=ORIENTED_EDGE('',*,*,#4939,.T.);
#6566=ORIENTED_EDGE('',*,*,#4933,.T.);
#6567=ORIENTED_EDGE('',*,*,#4937,.T.);
#6568=ORIENTED_EDGE('',*,*,#5141,.T.);
#6569=ORIENTED_EDGE('',*,*,#5005,.T.);
#6570=ORIENTED_EDGE('',*,*,#4999,.T.);
#6571=ORIENTED_EDGE('',*,*,#5003,.T.);
#6572=ORIENTED_EDGE('',*,*,#5142,.T.);
#6573=ORIENTED_EDGE('',*,*,#4928,.T.);
#6574=ORIENTED_EDGE('',*,*,#4922,.T.);
#6575=ORIENTED_EDGE('',*,*,#4926,.T.);
#6576=ORIENTED_EDGE('',*,*,#5143,.T.);
#6577=ORIENTED_EDGE('',*,*,#5016,.T.);
#6578=ORIENTED_EDGE('',*,*,#5010,.T.);
#6579=ORIENTED_EDGE('',*,*,#5014,.T.);
#6580=ORIENTED_EDGE('',*,*,#5144,.T.);
#6581=ORIENTED_EDGE('',*,*,#4917,.T.);
#6582=ORIENTED_EDGE('',*,*,#4911,.T.);
#6583=ORIENTED_EDGE('',*,*,#4915,.T.);
#6584=ORIENTED_EDGE('',*,*,#5145,.T.);
#6585=ORIENTED_EDGE('',*,*,#5027,.T.);
#6586=ORIENTED_EDGE('',*,*,#5021,.T.);
#6587=ORIENTED_EDGE('',*,*,#5025,.T.);
#6588=ORIENTED_EDGE('',*,*,#5146,.T.);
#6589=ORIENTED_EDGE('',*,*,#4906,.T.);
#6590=ORIENTED_EDGE('',*,*,#4900,.T.);
#6591=ORIENTED_EDGE('',*,*,#4904,.T.);
#6592=ORIENTED_EDGE('',*,*,#5147,.T.);
#6593=ORIENTED_EDGE('',*,*,#5038,.T.);
#6594=ORIENTED_EDGE('',*,*,#5032,.T.);
#6595=ORIENTED_EDGE('',*,*,#5036,.T.);
#6596=ORIENTED_EDGE('',*,*,#5148,.T.);
#6597=ORIENTED_EDGE('',*,*,#4895,.T.);
#6598=ORIENTED_EDGE('',*,*,#4889,.T.);
#6599=ORIENTED_EDGE('',*,*,#4893,.T.);
#6600=ORIENTED_EDGE('',*,*,#5149,.T.);
#6601=ORIENTED_EDGE('',*,*,#4884,.T.);
#6602=ORIENTED_EDGE('',*,*,#4878,.T.);
#6603=ORIENTED_EDGE('',*,*,#4882,.T.);
#6604=ORIENTED_EDGE('',*,*,#5150,.T.);
#6605=ORIENTED_EDGE('',*,*,#5060,.T.);
#6606=ORIENTED_EDGE('',*,*,#5054,.T.);
#6607=ORIENTED_EDGE('',*,*,#5058,.T.);
#6608=ORIENTED_EDGE('',*,*,#5151,.T.);
#6609=ORIENTED_EDGE('',*,*,#4873,.T.);
#6610=ORIENTED_EDGE('',*,*,#4867,.T.);
#6611=ORIENTED_EDGE('',*,*,#4871,.T.);
#6612=ORIENTED_EDGE('',*,*,#5152,.T.);
#6613=ORIENTED_EDGE('',*,*,#5071,.T.);
#6614=ORIENTED_EDGE('',*,*,#5065,.T.);
#6615=ORIENTED_EDGE('',*,*,#5069,.T.);
#6616=ORIENTED_EDGE('',*,*,#5153,.T.);
#6617=ORIENTED_EDGE('',*,*,#4862,.T.);
#6618=ORIENTED_EDGE('',*,*,#4856,.T.);
#6619=ORIENTED_EDGE('',*,*,#4860,.T.);
#6620=ORIENTED_EDGE('',*,*,#5154,.T.);
#6621=ORIENTED_EDGE('',*,*,#5082,.T.);
#6622=ORIENTED_EDGE('',*,*,#5076,.T.);
#6623=ORIENTED_EDGE('',*,*,#5080,.T.);
#6624=ORIENTED_EDGE('',*,*,#5155,.T.);
#6625=ORIENTED_EDGE('',*,*,#4851,.T.);
#6626=ORIENTED_EDGE('',*,*,#4845,.T.);
#6627=ORIENTED_EDGE('',*,*,#4849,.T.);
#6628=ORIENTED_EDGE('',*,*,#5156,.T.);
#6629=ORIENTED_EDGE('',*,*,#5093,.T.);
#6630=ORIENTED_EDGE('',*,*,#5087,.T.);
#6631=ORIENTED_EDGE('',*,*,#5091,.T.);
#6632=ORIENTED_EDGE('',*,*,#5157,.T.);
#6633=ORIENTED_EDGE('',*,*,#4840,.T.);
#6634=ORIENTED_EDGE('',*,*,#4834,.T.);
#6635=ORIENTED_EDGE('',*,*,#4838,.T.);
#6636=ORIENTED_EDGE('',*,*,#5158,.T.);
#6637=ORIENTED_EDGE('',*,*,#5104,.T.);
#6638=ORIENTED_EDGE('',*,*,#5098,.T.);
#6639=ORIENTED_EDGE('',*,*,#5102,.T.);
#6640=ORIENTED_EDGE('',*,*,#5159,.T.);
#6641=ORIENTED_EDGE('',*,*,#4829,.T.);
#6642=ORIENTED_EDGE('',*,*,#4823,.T.);
#6643=ORIENTED_EDGE('',*,*,#4827,.T.);
#6644=ORIENTED_EDGE('',*,*,#5160,.T.);
#6645=ORIENTED_EDGE('',*,*,#5115,.T.);
#6646=ORIENTED_EDGE('',*,*,#5109,.T.);
#6647=ORIENTED_EDGE('',*,*,#5113,.T.);
#6648=ORIENTED_EDGE('',*,*,#5161,.T.);
#6649=ORIENTED_EDGE('',*,*,#5162,.T.);
#6650=ORIENTED_EDGE('',*,*,#5163,.T.);
#6651=ORIENTED_EDGE('',*,*,#5164,.F.);
#6652=ORIENTED_EDGE('',*,*,#5165,.T.);
#6653=ORIENTED_EDGE('',*,*,#5163,.F.);
#6654=ORIENTED_EDGE('',*,*,#5165,.F.);
#6655=ORIENTED_EDGE('',*,*,#5166,.F.);
#6656=ORIENTED_EDGE('',*,*,#5167,.T.);
#6657=ORIENTED_EDGE('',*,*,#5162,.F.);
#6658=ORIENTED_EDGE('',*,*,#5167,.F.);
#6659=ORIENTED_EDGE('',*,*,#5168,.T.);
#6660=ORIENTED_EDGE('',*,*,#5169,.T.);
#6661=ORIENTED_EDGE('',*,*,#5132,.F.);
#6662=ORIENTED_EDGE('',*,*,#5170,.F.);
#6663=ORIENTED_EDGE('',*,*,#5171,.T.);
#6664=ORIENTED_EDGE('',*,*,#5170,.T.);
#6665=ORIENTED_EDGE('',*,*,#5131,.F.);
#6666=ORIENTED_EDGE('',*,*,#5172,.F.);
#6667=ORIENTED_EDGE('',*,*,#4819,.T.);
#6668=ORIENTED_EDGE('',*,*,#5161,.F.);
#6669=ORIENTED_EDGE('',*,*,#5112,.T.);
#6670=ORIENTED_EDGE('',*,*,#5117,.T.);
#6671=ORIENTED_EDGE('',*,*,#5116,.T.);
#6672=ORIENTED_EDGE('',*,*,#5160,.F.);
#6673=ORIENTED_EDGE('',*,*,#4826,.T.);
#6674=ORIENTED_EDGE('',*,*,#4831,.T.);
#6675=ORIENTED_EDGE('',*,*,#4830,.T.);
#6676=ORIENTED_EDGE('',*,*,#5159,.F.);
#6677=ORIENTED_EDGE('',*,*,#5101,.T.);
#6678=ORIENTED_EDGE('',*,*,#5106,.T.);
#6679=ORIENTED_EDGE('',*,*,#5105,.T.);
#6680=ORIENTED_EDGE('',*,*,#5158,.F.);
#6681=ORIENTED_EDGE('',*,*,#4837,.T.);
#6682=ORIENTED_EDGE('',*,*,#4842,.T.);
#6683=ORIENTED_EDGE('',*,*,#4841,.T.);
#6684=ORIENTED_EDGE('',*,*,#5157,.F.);
#6685=ORIENTED_EDGE('',*,*,#5090,.T.);
#6686=ORIENTED_EDGE('',*,*,#5095,.T.);
#6687=ORIENTED_EDGE('',*,*,#5094,.T.);
#6688=ORIENTED_EDGE('',*,*,#5156,.F.);
#6689=ORIENTED_EDGE('',*,*,#4848,.T.);
#6690=ORIENTED_EDGE('',*,*,#4853,.T.);
#6691=ORIENTED_EDGE('',*,*,#4852,.T.);
#6692=ORIENTED_EDGE('',*,*,#5155,.F.);
#6693=ORIENTED_EDGE('',*,*,#5079,.T.);
#6694=ORIENTED_EDGE('',*,*,#5084,.T.);
#6695=ORIENTED_EDGE('',*,*,#5083,.T.);
#6696=ORIENTED_EDGE('',*,*,#5154,.F.);
#6697=ORIENTED_EDGE('',*,*,#4859,.T.);
#6698=ORIENTED_EDGE('',*,*,#4864,.T.);
#6699=ORIENTED_EDGE('',*,*,#4863,.T.);
#6700=ORIENTED_EDGE('',*,*,#5153,.F.);
#6701=ORIENTED_EDGE('',*,*,#5068,.T.);
#6702=ORIENTED_EDGE('',*,*,#5073,.T.);
#6703=ORIENTED_EDGE('',*,*,#5072,.T.);
#6704=ORIENTED_EDGE('',*,*,#5152,.F.);
#6705=ORIENTED_EDGE('',*,*,#4870,.T.);
#6706=ORIENTED_EDGE('',*,*,#4875,.T.);
#6707=ORIENTED_EDGE('',*,*,#4874,.T.);
#6708=ORIENTED_EDGE('',*,*,#5151,.F.);
#6709=ORIENTED_EDGE('',*,*,#5057,.T.);
#6710=ORIENTED_EDGE('',*,*,#5062,.T.);
#6711=ORIENTED_EDGE('',*,*,#5061,.T.);
#6712=ORIENTED_EDGE('',*,*,#5150,.F.);
#6713=ORIENTED_EDGE('',*,*,#4881,.T.);
#6714=ORIENTED_EDGE('',*,*,#4886,.T.);
#6715=ORIENTED_EDGE('',*,*,#4885,.T.);
#6716=ORIENTED_EDGE('',*,*,#5149,.F.);
#6717=ORIENTED_EDGE('',*,*,#4892,.T.);
#6718=ORIENTED_EDGE('',*,*,#4897,.T.);
#6719=ORIENTED_EDGE('',*,*,#4896,.T.);
#6720=ORIENTED_EDGE('',*,*,#5148,.F.);
#6721=ORIENTED_EDGE('',*,*,#5035,.T.);
#6722=ORIENTED_EDGE('',*,*,#5040,.T.);
#6723=ORIENTED_EDGE('',*,*,#5039,.T.);
#6724=ORIENTED_EDGE('',*,*,#5147,.F.);
#6725=ORIENTED_EDGE('',*,*,#4903,.T.);
#6726=ORIENTED_EDGE('',*,*,#4908,.T.);
#6727=ORIENTED_EDGE('',*,*,#4907,.T.);
#6728=ORIENTED_EDGE('',*,*,#5146,.F.);
#6729=ORIENTED_EDGE('',*,*,#5024,.T.);
#6730=ORIENTED_EDGE('',*,*,#5029,.T.);
#6731=ORIENTED_EDGE('',*,*,#5028,.T.);
#6732=ORIENTED_EDGE('',*,*,#5145,.F.);
#6733=ORIENTED_EDGE('',*,*,#4914,.T.);
#6734=ORIENTED_EDGE('',*,*,#4919,.T.);
#6735=ORIENTED_EDGE('',*,*,#4918,.T.);
#6736=ORIENTED_EDGE('',*,*,#5144,.F.);
#6737=ORIENTED_EDGE('',*,*,#5013,.T.);
#6738=ORIENTED_EDGE('',*,*,#5018,.T.);
#6739=ORIENTED_EDGE('',*,*,#5017,.T.);
#6740=ORIENTED_EDGE('',*,*,#5143,.F.);
#6741=ORIENTED_EDGE('',*,*,#4925,.T.);
#6742=ORIENTED_EDGE('',*,*,#4930,.T.);
#6743=ORIENTED_EDGE('',*,*,#4929,.T.);
#6744=ORIENTED_EDGE('',*,*,#5142,.F.);
#6745=ORIENTED_EDGE('',*,*,#5002,.T.);
#6746=ORIENTED_EDGE('',*,*,#5007,.T.);
#6747=ORIENTED_EDGE('',*,*,#5006,.T.);
#6748=ORIENTED_EDGE('',*,*,#5141,.F.);
#6749=ORIENTED_EDGE('',*,*,#4936,.T.);
#6750=ORIENTED_EDGE('',*,*,#4941,.T.);
#6751=ORIENTED_EDGE('',*,*,#4940,.T.);
#6752=ORIENTED_EDGE('',*,*,#5140,.F.);
#6753=ORIENTED_EDGE('',*,*,#4991,.T.);
#6754=ORIENTED_EDGE('',*,*,#4996,.T.);
#6755=ORIENTED_EDGE('',*,*,#4995,.T.);
#6756=ORIENTED_EDGE('',*,*,#5139,.F.);
#6757=ORIENTED_EDGE('',*,*,#4947,.T.);
#6758=ORIENTED_EDGE('',*,*,#4952,.T.);
#6759=ORIENTED_EDGE('',*,*,#4951,.T.);
#6760=ORIENTED_EDGE('',*,*,#5138,.F.);
#6761=ORIENTED_EDGE('',*,*,#4980,.T.);
#6762=ORIENTED_EDGE('',*,*,#4985,.T.);
#6763=ORIENTED_EDGE('',*,*,#4984,.T.);
#6764=ORIENTED_EDGE('',*,*,#5137,.F.);
#6765=ORIENTED_EDGE('',*,*,#4958,.T.);
#6766=ORIENTED_EDGE('',*,*,#4963,.T.);
#6767=ORIENTED_EDGE('',*,*,#4962,.T.);
#6768=ORIENTED_EDGE('',*,*,#5136,.F.);
#6769=ORIENTED_EDGE('',*,*,#4969,.T.);
#6770=ORIENTED_EDGE('',*,*,#4974,.T.);
#6771=ORIENTED_EDGE('',*,*,#4973,.T.);
#6772=ORIENTED_EDGE('',*,*,#5135,.F.);
#6773=ORIENTED_EDGE('',*,*,#5046,.T.);
#6774=ORIENTED_EDGE('',*,*,#5051,.T.);
#6775=ORIENTED_EDGE('',*,*,#5050,.T.);
#6776=ORIENTED_EDGE('',*,*,#5134,.F.);
#6777=ORIENTED_EDGE('',*,*,#5173,.F.);
#6778=ORIENTED_EDGE('',*,*,#5174,.T.);
#6779=ORIENTED_EDGE('',*,*,#5172,.T.);
#6780=ORIENTED_EDGE('',*,*,#5130,.F.);
#6781=ORIENTED_EDGE('',*,*,#5123,.T.);
#6782=ORIENTED_EDGE('',*,*,#5128,.T.);
#6783=ORIENTED_EDGE('',*,*,#5127,.T.);
#6784=ORIENTED_EDGE('',*,*,#5129,.F.);
#6785=ORIENTED_EDGE('',*,*,#4815,.T.);
#6786=ORIENTED_EDGE('',*,*,#4820,.T.);
#6787=ORIENTED_EDGE('',*,*,#5175,.T.);
#6788=ORIENTED_EDGE('',*,*,#5173,.T.);
#6789=ORIENTED_EDGE('',*,*,#5133,.F.);
#6790=ORIENTED_EDGE('',*,*,#5169,.F.);
#6791=ORIENTED_EDGE('',*,*,#5175,.F.);
#6792=ORIENTED_EDGE('',*,*,#5168,.F.);
#6793=ORIENTED_EDGE('',*,*,#5171,.F.);
#6794=ORIENTED_EDGE('',*,*,#5174,.F.);
#6795=ORIENTED_EDGE('',*,*,#5164,.T.);
#6796=ORIENTED_EDGE('',*,*,#5166,.T.);
#6797=ORIENTED_EDGE('',*,*,#5176,.T.);
#6798=ORIENTED_EDGE('',*,*,#5177,.T.);
#6799=ORIENTED_EDGE('',*,*,#5178,.F.);
#6800=ORIENTED_EDGE('',*,*,#5179,.F.);
#6801=ORIENTED_EDGE('',*,*,#5180,.T.);
#6802=ORIENTED_EDGE('',*,*,#5179,.T.);
#6803=ORIENTED_EDGE('',*,*,#5181,.F.);
#6804=ORIENTED_EDGE('',*,*,#5182,.F.);
#6805=ORIENTED_EDGE('',*,*,#5183,.T.);
#6806=ORIENTED_EDGE('',*,*,#5182,.T.);
#6807=ORIENTED_EDGE('',*,*,#5184,.F.);
#6808=ORIENTED_EDGE('',*,*,#5185,.F.);
#6809=ORIENTED_EDGE('',*,*,#5186,.T.);
#6810=ORIENTED_EDGE('',*,*,#5185,.T.);
#6811=ORIENTED_EDGE('',*,*,#5187,.F.);
#6812=ORIENTED_EDGE('',*,*,#5177,.F.);
#6813=ORIENTED_EDGE('',*,*,#5187,.T.);
#6814=ORIENTED_EDGE('',*,*,#5184,.T.);
#6815=ORIENTED_EDGE('',*,*,#5181,.T.);
#6816=ORIENTED_EDGE('',*,*,#5178,.T.);
#6817=ORIENTED_EDGE('',*,*,#5186,.F.);
#6818=ORIENTED_EDGE('',*,*,#5176,.F.);
#6819=ORIENTED_EDGE('',*,*,#5180,.F.);
#6820=ORIENTED_EDGE('',*,*,#5183,.F.);
#6821=ORIENTED_EDGE('',*,*,#5188,.T.);
#6822=ORIENTED_EDGE('',*,*,#5189,.T.);
#6823=ORIENTED_EDGE('',*,*,#5190,.F.);
#6824=ORIENTED_EDGE('',*,*,#5191,.F.);
#6825=ORIENTED_EDGE('',*,*,#5192,.T.);
#6826=ORIENTED_EDGE('',*,*,#5191,.T.);
#6827=ORIENTED_EDGE('',*,*,#5193,.F.);
#6828=ORIENTED_EDGE('',*,*,#5194,.F.);
#6829=ORIENTED_EDGE('',*,*,#5195,.T.);
#6830=ORIENTED_EDGE('',*,*,#5194,.T.);
#6831=ORIENTED_EDGE('',*,*,#5196,.F.);
#6832=ORIENTED_EDGE('',*,*,#5197,.F.);
#6833=ORIENTED_EDGE('',*,*,#5198,.T.);
#6834=ORIENTED_EDGE('',*,*,#5197,.T.);
#6835=ORIENTED_EDGE('',*,*,#5199,.F.);
#6836=ORIENTED_EDGE('',*,*,#5189,.F.);
#6837=ORIENTED_EDGE('',*,*,#5199,.T.);
#6838=ORIENTED_EDGE('',*,*,#5196,.T.);
#6839=ORIENTED_EDGE('',*,*,#5193,.T.);
#6840=ORIENTED_EDGE('',*,*,#5190,.T.);
#6841=ORIENTED_EDGE('',*,*,#5198,.F.);
#6842=ORIENTED_EDGE('',*,*,#5188,.F.);
#6843=ORIENTED_EDGE('',*,*,#5192,.F.);
#6844=ORIENTED_EDGE('',*,*,#5195,.F.);
#6845=ORIENTED_EDGE('',*,*,#5200,.T.);
#6846=ORIENTED_EDGE('',*,*,#5201,.T.);
#6847=ORIENTED_EDGE('',*,*,#5202,.F.);
#6848=ORIENTED_EDGE('',*,*,#5203,.F.);
#6849=ORIENTED_EDGE('',*,*,#5204,.T.);
#6850=ORIENTED_EDGE('',*,*,#5203,.T.);
#6851=ORIENTED_EDGE('',*,*,#5205,.F.);
#6852=ORIENTED_EDGE('',*,*,#5206,.F.);
#6853=ORIENTED_EDGE('',*,*,#5207,.T.);
#6854=ORIENTED_EDGE('',*,*,#5206,.T.);
#6855=ORIENTED_EDGE('',*,*,#5208,.F.);
#6856=ORIENTED_EDGE('',*,*,#5209,.F.);
#6857=ORIENTED_EDGE('',*,*,#5210,.T.);
#6858=ORIENTED_EDGE('',*,*,#5209,.T.);
#6859=ORIENTED_EDGE('',*,*,#5211,.F.);
#6860=ORIENTED_EDGE('',*,*,#5201,.F.);
#6861=ORIENTED_EDGE('',*,*,#5211,.T.);
#6862=ORIENTED_EDGE('',*,*,#5208,.T.);
#6863=ORIENTED_EDGE('',*,*,#5205,.T.);
#6864=ORIENTED_EDGE('',*,*,#5202,.T.);
#6865=ORIENTED_EDGE('',*,*,#5210,.F.);
#6866=ORIENTED_EDGE('',*,*,#5200,.F.);
#6867=ORIENTED_EDGE('',*,*,#5204,.F.);
#6868=ORIENTED_EDGE('',*,*,#5207,.F.);
#6869=ORIENTED_EDGE('',*,*,#5212,.T.);
#6870=ORIENTED_EDGE('',*,*,#5213,.T.);
#6871=ORIENTED_EDGE('',*,*,#5214,.F.);
#6872=ORIENTED_EDGE('',*,*,#5215,.F.);
#6873=ORIENTED_EDGE('',*,*,#5216,.T.);
#6874=ORIENTED_EDGE('',*,*,#5215,.T.);
#6875=ORIENTED_EDGE('',*,*,#5217,.F.);
#6876=ORIENTED_EDGE('',*,*,#5218,.F.);
#6877=ORIENTED_EDGE('',*,*,#5219,.T.);
#6878=ORIENTED_EDGE('',*,*,#5218,.T.);
#6879=ORIENTED_EDGE('',*,*,#5220,.F.);
#6880=ORIENTED_EDGE('',*,*,#5221,.F.);
#6881=ORIENTED_EDGE('',*,*,#5222,.T.);
#6882=ORIENTED_EDGE('',*,*,#5221,.T.);
#6883=ORIENTED_EDGE('',*,*,#5223,.F.);
#6884=ORIENTED_EDGE('',*,*,#5213,.F.);
#6885=ORIENTED_EDGE('',*,*,#5223,.T.);
#6886=ORIENTED_EDGE('',*,*,#5220,.T.);
#6887=ORIENTED_EDGE('',*,*,#5217,.T.);
#6888=ORIENTED_EDGE('',*,*,#5214,.T.);
#6889=ORIENTED_EDGE('',*,*,#5222,.F.);
#6890=ORIENTED_EDGE('',*,*,#5212,.F.);
#6891=ORIENTED_EDGE('',*,*,#5216,.F.);
#6892=ORIENTED_EDGE('',*,*,#5219,.F.);
#6893=ORIENTED_EDGE('',*,*,#5224,.F.);
#6894=ORIENTED_EDGE('',*,*,#5225,.T.);
#6895=ORIENTED_EDGE('',*,*,#5226,.F.);
#6896=ORIENTED_EDGE('',*,*,#5225,.F.);
#6897=ORIENTED_EDGE('',*,*,#5224,.T.);
#6898=ORIENTED_EDGE('',*,*,#5227,.F.);
#6899=ORIENTED_EDGE('',*,*,#5228,.F.);
#6900=ORIENTED_EDGE('',*,*,#5229,.T.);
#6901=ORIENTED_EDGE('',*,*,#5230,.F.);
#6902=ORIENTED_EDGE('',*,*,#5229,.F.);
#6903=ORIENTED_EDGE('',*,*,#5228,.T.);
#6904=ORIENTED_EDGE('',*,*,#5231,.F.);
#6905=ORIENTED_EDGE('',*,*,#5232,.F.);
#6906=ORIENTED_EDGE('',*,*,#5233,.T.);
#6907=ORIENTED_EDGE('',*,*,#5234,.F.);
#6908=ORIENTED_EDGE('',*,*,#5233,.F.);
#6909=ORIENTED_EDGE('',*,*,#5232,.T.);
#6910=ORIENTED_EDGE('',*,*,#5235,.F.);
#6911=ORIENTED_EDGE('',*,*,#5236,.F.);
#6912=ORIENTED_EDGE('',*,*,#5237,.T.);
#6913=ORIENTED_EDGE('',*,*,#5238,.F.);
#6914=ORIENTED_EDGE('',*,*,#5237,.F.);
#6915=ORIENTED_EDGE('',*,*,#5236,.T.);
#6916=ORIENTED_EDGE('',*,*,#5239,.F.);
#6917=ORIENTED_EDGE('',*,*,#5240,.F.);
#6918=ORIENTED_EDGE('',*,*,#5241,.T.);
#6919=ORIENTED_EDGE('',*,*,#5227,.T.);
#6920=ORIENTED_EDGE('',*,*,#5241,.F.);
#6921=ORIENTED_EDGE('',*,*,#5242,.F.);
#6922=ORIENTED_EDGE('',*,*,#5243,.T.);
#6923=ORIENTED_EDGE('',*,*,#5231,.T.);
#6924=ORIENTED_EDGE('',*,*,#5243,.F.);
#6925=ORIENTED_EDGE('',*,*,#5244,.F.);
#6926=ORIENTED_EDGE('',*,*,#5245,.T.);
#6927=ORIENTED_EDGE('',*,*,#5235,.T.);
#6928=ORIENTED_EDGE('',*,*,#5245,.F.);
#6929=ORIENTED_EDGE('',*,*,#5246,.F.);
#6930=ORIENTED_EDGE('',*,*,#5247,.T.);
#6931=ORIENTED_EDGE('',*,*,#5239,.T.);
#6932=ORIENTED_EDGE('',*,*,#5247,.F.);
#6933=ORIENTED_EDGE('',*,*,#5248,.T.);
#6934=ORIENTED_EDGE('',*,*,#5249,.T.);
#6935=ORIENTED_EDGE('',*,*,#5250,.F.);
#6936=ORIENTED_EDGE('',*,*,#5251,.F.);
#6937=ORIENTED_EDGE('',*,*,#5252,.T.);
#6938=ORIENTED_EDGE('',*,*,#5251,.T.);
#6939=ORIENTED_EDGE('',*,*,#5253,.F.);
#6940=ORIENTED_EDGE('',*,*,#5254,.F.);
#6941=ORIENTED_EDGE('',*,*,#5255,.T.);
#6942=ORIENTED_EDGE('',*,*,#5254,.T.);
#6943=ORIENTED_EDGE('',*,*,#5256,.F.);
#6944=ORIENTED_EDGE('',*,*,#5257,.F.);
#6945=ORIENTED_EDGE('',*,*,#5258,.T.);
#6946=ORIENTED_EDGE('',*,*,#5257,.T.);
#6947=ORIENTED_EDGE('',*,*,#5259,.F.);
#6948=ORIENTED_EDGE('',*,*,#5260,.F.);
#6949=ORIENTED_EDGE('',*,*,#5261,.T.);
#6950=ORIENTED_EDGE('',*,*,#5260,.T.);
#6951=ORIENTED_EDGE('',*,*,#5262,.F.);
#6952=ORIENTED_EDGE('',*,*,#5263,.F.);
#6953=ORIENTED_EDGE('',*,*,#5238,.T.);
#6954=ORIENTED_EDGE('',*,*,#5234,.T.);
#6955=ORIENTED_EDGE('',*,*,#5230,.T.);
#6956=ORIENTED_EDGE('',*,*,#5226,.T.);
#6957=ORIENTED_EDGE('',*,*,#5264,.T.);
#6958=ORIENTED_EDGE('',*,*,#5263,.T.);
#6959=ORIENTED_EDGE('',*,*,#5265,.F.);
#6960=ORIENTED_EDGE('',*,*,#5266,.F.);
#6961=ORIENTED_EDGE('',*,*,#5267,.T.);
#6962=ORIENTED_EDGE('',*,*,#5266,.T.);
#6963=ORIENTED_EDGE('',*,*,#5268,.F.);
#6964=ORIENTED_EDGE('',*,*,#5269,.F.);
#6965=ORIENTED_EDGE('',*,*,#5270,.T.);
#6966=ORIENTED_EDGE('',*,*,#5269,.T.);
#6967=ORIENTED_EDGE('',*,*,#5271,.F.);
#6968=ORIENTED_EDGE('',*,*,#5272,.F.);
#6969=ORIENTED_EDGE('',*,*,#5273,.T.);
#6970=ORIENTED_EDGE('',*,*,#5272,.T.);
#6971=ORIENTED_EDGE('',*,*,#5274,.F.);
#6972=ORIENTED_EDGE('',*,*,#5275,.F.);
#6973=ORIENTED_EDGE('',*,*,#5276,.T.);
#6974=ORIENTED_EDGE('',*,*,#5275,.T.);
#6975=ORIENTED_EDGE('',*,*,#5277,.F.);
#6976=ORIENTED_EDGE('',*,*,#5278,.F.);
#6977=ORIENTED_EDGE('',*,*,#5279,.T.);
#6978=ORIENTED_EDGE('',*,*,#5278,.T.);
#6979=ORIENTED_EDGE('',*,*,#5280,.F.);
#6980=ORIENTED_EDGE('',*,*,#5281,.F.);
#6981=ORIENTED_EDGE('',*,*,#5240,.T.);
#6982=ORIENTED_EDGE('',*,*,#5242,.T.);
#6983=ORIENTED_EDGE('',*,*,#5244,.T.);
#6984=ORIENTED_EDGE('',*,*,#5246,.T.);
#6985=ORIENTED_EDGE('',*,*,#5282,.T.);
#6986=ORIENTED_EDGE('',*,*,#5281,.T.);
#6987=ORIENTED_EDGE('',*,*,#5283,.F.);
#6988=ORIENTED_EDGE('',*,*,#5249,.F.);
#6989=ORIENTED_EDGE('',*,*,#5283,.T.);
#6990=ORIENTED_EDGE('',*,*,#5280,.T.);
#6991=ORIENTED_EDGE('',*,*,#5277,.T.);
#6992=ORIENTED_EDGE('',*,*,#5274,.T.);
#6993=ORIENTED_EDGE('',*,*,#5271,.T.);
#6994=ORIENTED_EDGE('',*,*,#5268,.T.);
#6995=ORIENTED_EDGE('',*,*,#5265,.T.);
#6996=ORIENTED_EDGE('',*,*,#5262,.T.);
#6997=ORIENTED_EDGE('',*,*,#5259,.T.);
#6998=ORIENTED_EDGE('',*,*,#5256,.T.);
#6999=ORIENTED_EDGE('',*,*,#5253,.T.);
#7000=ORIENTED_EDGE('',*,*,#5250,.T.);
#7001=ORIENTED_EDGE('',*,*,#5282,.F.);
#7002=ORIENTED_EDGE('',*,*,#5248,.F.);
#7003=ORIENTED_EDGE('',*,*,#5252,.F.);
#7004=ORIENTED_EDGE('',*,*,#5255,.F.);
#7005=ORIENTED_EDGE('',*,*,#5258,.F.);
#7006=ORIENTED_EDGE('',*,*,#5261,.F.);
#7007=ORIENTED_EDGE('',*,*,#5264,.F.);
#7008=ORIENTED_EDGE('',*,*,#5267,.F.);
#7009=ORIENTED_EDGE('',*,*,#5270,.F.);
#7010=ORIENTED_EDGE('',*,*,#5273,.F.);
#7011=ORIENTED_EDGE('',*,*,#5276,.F.);
#7012=ORIENTED_EDGE('',*,*,#5279,.F.);
#7013=ORIENTED_EDGE('',*,*,#5284,.F.);
#7014=ORIENTED_EDGE('',*,*,#5285,.T.);
#7015=ORIENTED_EDGE('',*,*,#5286,.F.);
#7016=ORIENTED_EDGE('',*,*,#5287,.F.);
#7017=ORIENTED_EDGE('',*,*,#5288,.F.);
#7018=ORIENTED_EDGE('',*,*,#5289,.T.);
#7019=ORIENTED_EDGE('',*,*,#5290,.F.);
#7020=ORIENTED_EDGE('',*,*,#5285,.F.);
#7021=ORIENTED_EDGE('',*,*,#5291,.F.);
#7022=ORIENTED_EDGE('',*,*,#5292,.T.);
#7023=ORIENTED_EDGE('',*,*,#5293,.F.);
#7024=ORIENTED_EDGE('',*,*,#5289,.F.);
#7025=ORIENTED_EDGE('',*,*,#5294,.F.);
#7026=ORIENTED_EDGE('',*,*,#5295,.T.);
#7027=ORIENTED_EDGE('',*,*,#5296,.F.);
#7028=ORIENTED_EDGE('',*,*,#5292,.F.);
#7029=ORIENTED_EDGE('',*,*,#5297,.F.);
#7030=ORIENTED_EDGE('',*,*,#5298,.T.);
#7031=ORIENTED_EDGE('',*,*,#5299,.F.);
#7032=ORIENTED_EDGE('',*,*,#5295,.F.);
#7033=ORIENTED_EDGE('',*,*,#5300,.F.);
#7034=ORIENTED_EDGE('',*,*,#5301,.T.);
#7035=ORIENTED_EDGE('',*,*,#5302,.F.);
#7036=ORIENTED_EDGE('',*,*,#5298,.F.);
#7037=ORIENTED_EDGE('',*,*,#5303,.F.);
#7038=ORIENTED_EDGE('',*,*,#5304,.T.);
#7039=ORIENTED_EDGE('',*,*,#5305,.F.);
#7040=ORIENTED_EDGE('',*,*,#5301,.F.);
#7041=ORIENTED_EDGE('',*,*,#5306,.F.);
#7042=ORIENTED_EDGE('',*,*,#5307,.T.);
#7043=ORIENTED_EDGE('',*,*,#5308,.F.);
#7044=ORIENTED_EDGE('',*,*,#5304,.F.);
#7045=ORIENTED_EDGE('',*,*,#5309,.F.);
#7046=ORIENTED_EDGE('',*,*,#5310,.F.);
#7047=ORIENTED_EDGE('',*,*,#5311,.F.);
#7048=ORIENTED_EDGE('',*,*,#5307,.F.);
#7049=ORIENTED_EDGE('',*,*,#5312,.F.);
#7050=ORIENTED_EDGE('',*,*,#5313,.T.);
#7051=ORIENTED_EDGE('',*,*,#5314,.F.);
#7052=ORIENTED_EDGE('',*,*,#5315,.F.);
#7053=ORIENTED_EDGE('',*,*,#5316,.F.);
#7054=ORIENTED_EDGE('',*,*,#5317,.T.);
#7055=ORIENTED_EDGE('',*,*,#5318,.F.);
#7056=ORIENTED_EDGE('',*,*,#5313,.F.);
#7057=ORIENTED_EDGE('',*,*,#5319,.F.);
#7058=ORIENTED_EDGE('',*,*,#5320,.T.);
#7059=ORIENTED_EDGE('',*,*,#5321,.F.);
#7060=ORIENTED_EDGE('',*,*,#5317,.F.);
#7061=ORIENTED_EDGE('',*,*,#5322,.F.);
#7062=ORIENTED_EDGE('',*,*,#5323,.T.);
#7063=ORIENTED_EDGE('',*,*,#5324,.F.);
#7064=ORIENTED_EDGE('',*,*,#5320,.F.);
#7065=ORIENTED_EDGE('',*,*,#5325,.F.);
#7066=ORIENTED_EDGE('',*,*,#5326,.T.);
#7067=ORIENTED_EDGE('',*,*,#5327,.F.);
#7068=ORIENTED_EDGE('',*,*,#5323,.F.);
#7069=ORIENTED_EDGE('',*,*,#5328,.F.);
#7070=ORIENTED_EDGE('',*,*,#5329,.T.);
#7071=ORIENTED_EDGE('',*,*,#5330,.F.);
#7072=ORIENTED_EDGE('',*,*,#5326,.F.);
#7073=ORIENTED_EDGE('',*,*,#5331,.F.);
#7074=ORIENTED_EDGE('',*,*,#5332,.T.);
#7075=ORIENTED_EDGE('',*,*,#5333,.F.);
#7076=ORIENTED_EDGE('',*,*,#5329,.F.);
#7077=ORIENTED_EDGE('',*,*,#5334,.F.);
#7078=ORIENTED_EDGE('',*,*,#5335,.T.);
#7079=ORIENTED_EDGE('',*,*,#5336,.F.);
#7080=ORIENTED_EDGE('',*,*,#5332,.F.);
#7081=ORIENTED_EDGE('',*,*,#5337,.F.);
#7082=ORIENTED_EDGE('',*,*,#5338,.F.);
#7083=ORIENTED_EDGE('',*,*,#5339,.F.);
#7084=ORIENTED_EDGE('',*,*,#5335,.F.);
#7085=ORIENTED_EDGE('',*,*,#5340,.F.);
#7086=ORIENTED_EDGE('',*,*,#5341,.T.);
#7087=ORIENTED_EDGE('',*,*,#5342,.F.);
#7088=ORIENTED_EDGE('',*,*,#5343,.F.);
#7089=ORIENTED_EDGE('',*,*,#5344,.F.);
#7090=ORIENTED_EDGE('',*,*,#5345,.T.);
#7091=ORIENTED_EDGE('',*,*,#5346,.F.);
#7092=ORIENTED_EDGE('',*,*,#5341,.F.);
#7093=ORIENTED_EDGE('',*,*,#5347,.F.);
#7094=ORIENTED_EDGE('',*,*,#5348,.T.);
#7095=ORIENTED_EDGE('',*,*,#5349,.F.);
#7096=ORIENTED_EDGE('',*,*,#5345,.F.);
#7097=ORIENTED_EDGE('',*,*,#5350,.F.);
#7098=ORIENTED_EDGE('',*,*,#5351,.T.);
#7099=ORIENTED_EDGE('',*,*,#5352,.F.);
#7100=ORIENTED_EDGE('',*,*,#5348,.F.);
#7101=ORIENTED_EDGE('',*,*,#5353,.F.);
#7102=ORIENTED_EDGE('',*,*,#5354,.T.);
#7103=ORIENTED_EDGE('',*,*,#5355,.F.);
#7104=ORIENTED_EDGE('',*,*,#5351,.F.);
#7105=ORIENTED_EDGE('',*,*,#5356,.F.);
#7106=ORIENTED_EDGE('',*,*,#5357,.T.);
#7107=ORIENTED_EDGE('',*,*,#5358,.F.);
#7108=ORIENTED_EDGE('',*,*,#5354,.F.);
#7109=ORIENTED_EDGE('',*,*,#5359,.F.);
#7110=ORIENTED_EDGE('',*,*,#5360,.T.);
#7111=ORIENTED_EDGE('',*,*,#5361,.F.);
#7112=ORIENTED_EDGE('',*,*,#5357,.F.);
#7113=ORIENTED_EDGE('',*,*,#5362,.F.);
#7114=ORIENTED_EDGE('',*,*,#5363,.T.);
#7115=ORIENTED_EDGE('',*,*,#5364,.F.);
#7116=ORIENTED_EDGE('',*,*,#5360,.F.);
#7117=ORIENTED_EDGE('',*,*,#5365,.F.);
#7118=ORIENTED_EDGE('',*,*,#5366,.F.);
#7119=ORIENTED_EDGE('',*,*,#5367,.F.);
#7120=ORIENTED_EDGE('',*,*,#5363,.F.);
#7121=ORIENTED_EDGE('',*,*,#5368,.F.);
#7122=ORIENTED_EDGE('',*,*,#5369,.T.);
#7123=ORIENTED_EDGE('',*,*,#5370,.F.);
#7124=ORIENTED_EDGE('',*,*,#5371,.F.);
#7125=ORIENTED_EDGE('',*,*,#5372,.F.);
#7126=ORIENTED_EDGE('',*,*,#5373,.T.);
#7127=ORIENTED_EDGE('',*,*,#5374,.F.);
#7128=ORIENTED_EDGE('',*,*,#5369,.F.);
#7129=ORIENTED_EDGE('',*,*,#5375,.F.);
#7130=ORIENTED_EDGE('',*,*,#5376,.T.);
#7131=ORIENTED_EDGE('',*,*,#5377,.F.);
#7132=ORIENTED_EDGE('',*,*,#5373,.F.);
#7133=ORIENTED_EDGE('',*,*,#5378,.F.);
#7134=ORIENTED_EDGE('',*,*,#5379,.T.);
#7135=ORIENTED_EDGE('',*,*,#5380,.F.);
#7136=ORIENTED_EDGE('',*,*,#5376,.F.);
#7137=ORIENTED_EDGE('',*,*,#5381,.F.);
#7138=ORIENTED_EDGE('',*,*,#5382,.T.);
#7139=ORIENTED_EDGE('',*,*,#5383,.F.);
#7140=ORIENTED_EDGE('',*,*,#5379,.F.);
#7141=ORIENTED_EDGE('',*,*,#5384,.F.);
#7142=ORIENTED_EDGE('',*,*,#5385,.T.);
#7143=ORIENTED_EDGE('',*,*,#5386,.F.);
#7144=ORIENTED_EDGE('',*,*,#5382,.F.);
#7145=ORIENTED_EDGE('',*,*,#5387,.F.);
#7146=ORIENTED_EDGE('',*,*,#5388,.T.);
#7147=ORIENTED_EDGE('',*,*,#5389,.F.);
#7148=ORIENTED_EDGE('',*,*,#5385,.F.);
#7149=ORIENTED_EDGE('',*,*,#5390,.F.);
#7150=ORIENTED_EDGE('',*,*,#5391,.T.);
#7151=ORIENTED_EDGE('',*,*,#5392,.F.);
#7152=ORIENTED_EDGE('',*,*,#5388,.F.);
#7153=ORIENTED_EDGE('',*,*,#5393,.F.);
#7154=ORIENTED_EDGE('',*,*,#5394,.F.);
#7155=ORIENTED_EDGE('',*,*,#5395,.F.);
#7156=ORIENTED_EDGE('',*,*,#5391,.F.);
#7157=ORIENTED_EDGE('',*,*,#5396,.F.);
#7158=ORIENTED_EDGE('',*,*,#5397,.T.);
#7159=ORIENTED_EDGE('',*,*,#5398,.F.);
#7160=ORIENTED_EDGE('',*,*,#5397,.F.);
#7161=ORIENTED_EDGE('',*,*,#5310,.T.);
#7162=ORIENTED_EDGE('',*,*,#5399,.T.);
#7163=ORIENTED_EDGE('',*,*,#5400,.T.);
#7164=ORIENTED_EDGE('',*,*,#5401,.F.);
#7165=ORIENTED_EDGE('',*,*,#5287,.T.);
#7166=ORIENTED_EDGE('',*,*,#5402,.F.);
#7167=ORIENTED_EDGE('',*,*,#5403,.F.);
#7168=ORIENTED_EDGE('',*,*,#5404,.T.);
#7169=ORIENTED_EDGE('',*,*,#5338,.T.);
#7170=ORIENTED_EDGE('',*,*,#5405,.T.);
#7171=ORIENTED_EDGE('',*,*,#5403,.T.);
#7172=ORIENTED_EDGE('',*,*,#5406,.F.);
#7173=ORIENTED_EDGE('',*,*,#5315,.T.);
#7174=ORIENTED_EDGE('',*,*,#5407,.F.);
#7175=ORIENTED_EDGE('',*,*,#5408,.F.);
#7176=ORIENTED_EDGE('',*,*,#5409,.T.);
#7177=ORIENTED_EDGE('',*,*,#5366,.T.);
#7178=ORIENTED_EDGE('',*,*,#5410,.T.);
#7179=ORIENTED_EDGE('',*,*,#5408,.T.);
#7180=ORIENTED_EDGE('',*,*,#5411,.F.);
#7181=ORIENTED_EDGE('',*,*,#5343,.T.);
#7182=ORIENTED_EDGE('',*,*,#5412,.F.);
#7183=ORIENTED_EDGE('',*,*,#5413,.F.);
#7184=ORIENTED_EDGE('',*,*,#5414,.T.);
#7185=ORIENTED_EDGE('',*,*,#5394,.T.);
#7186=ORIENTED_EDGE('',*,*,#5415,.T.);
#7187=ORIENTED_EDGE('',*,*,#5413,.T.);
#7188=ORIENTED_EDGE('',*,*,#5416,.F.);
#7189=ORIENTED_EDGE('',*,*,#5371,.T.);
#7190=ORIENTED_EDGE('',*,*,#5417,.F.);
#7191=ORIENTED_EDGE('',*,*,#5400,.F.);
#7192=ORIENTED_EDGE('',*,*,#5418,.T.);
#7193=ORIENTED_EDGE('',*,*,#5286,.T.);
#7194=ORIENTED_EDGE('',*,*,#5290,.T.);
#7195=ORIENTED_EDGE('',*,*,#5293,.T.);
#7196=ORIENTED_EDGE('',*,*,#5296,.T.);
#7197=ORIENTED_EDGE('',*,*,#5299,.T.);
#7198=ORIENTED_EDGE('',*,*,#5302,.T.);
#7199=ORIENTED_EDGE('',*,*,#5305,.T.);
#7200=ORIENTED_EDGE('',*,*,#5308,.T.);
#7201=ORIENTED_EDGE('',*,*,#5311,.T.);
#7202=ORIENTED_EDGE('',*,*,#5401,.T.);
#7203=ORIENTED_EDGE('',*,*,#5417,.T.);
#7204=ORIENTED_EDGE('',*,*,#5370,.T.);
#7205=ORIENTED_EDGE('',*,*,#5374,.T.);
#7206=ORIENTED_EDGE('',*,*,#5377,.T.);
#7207=ORIENTED_EDGE('',*,*,#5380,.T.);
#7208=ORIENTED_EDGE('',*,*,#5383,.T.);
#7209=ORIENTED_EDGE('',*,*,#5386,.T.);
#7210=ORIENTED_EDGE('',*,*,#5389,.T.);
#7211=ORIENTED_EDGE('',*,*,#5392,.T.);
#7212=ORIENTED_EDGE('',*,*,#5395,.T.);
#7213=ORIENTED_EDGE('',*,*,#5416,.T.);
#7214=ORIENTED_EDGE('',*,*,#5412,.T.);
#7215=ORIENTED_EDGE('',*,*,#5342,.T.);
#7216=ORIENTED_EDGE('',*,*,#5346,.T.);
#7217=ORIENTED_EDGE('',*,*,#5349,.T.);
#7218=ORIENTED_EDGE('',*,*,#5352,.T.);
#7219=ORIENTED_EDGE('',*,*,#5355,.T.);
#7220=ORIENTED_EDGE('',*,*,#5358,.T.);
#7221=ORIENTED_EDGE('',*,*,#5361,.T.);
#7222=ORIENTED_EDGE('',*,*,#5364,.T.);
#7223=ORIENTED_EDGE('',*,*,#5367,.T.);
#7224=ORIENTED_EDGE('',*,*,#5411,.T.);
#7225=ORIENTED_EDGE('',*,*,#5407,.T.);
#7226=ORIENTED_EDGE('',*,*,#5314,.T.);
#7227=ORIENTED_EDGE('',*,*,#5318,.T.);
#7228=ORIENTED_EDGE('',*,*,#5321,.T.);
#7229=ORIENTED_EDGE('',*,*,#5324,.T.);
#7230=ORIENTED_EDGE('',*,*,#5327,.T.);
#7231=ORIENTED_EDGE('',*,*,#5330,.T.);
#7232=ORIENTED_EDGE('',*,*,#5333,.T.);
#7233=ORIENTED_EDGE('',*,*,#5336,.T.);
#7234=ORIENTED_EDGE('',*,*,#5339,.T.);
#7235=ORIENTED_EDGE('',*,*,#5406,.T.);
#7236=ORIENTED_EDGE('',*,*,#5402,.T.);
#7237=ORIENTED_EDGE('',*,*,#5398,.T.);
#7238=ORIENTED_EDGE('',*,*,#5284,.T.);
#7239=ORIENTED_EDGE('',*,*,#5404,.F.);
#7240=ORIENTED_EDGE('',*,*,#5405,.F.);
#7241=ORIENTED_EDGE('',*,*,#5337,.T.);
#7242=ORIENTED_EDGE('',*,*,#5334,.T.);
#7243=ORIENTED_EDGE('',*,*,#5331,.T.);
#7244=ORIENTED_EDGE('',*,*,#5328,.T.);
#7245=ORIENTED_EDGE('',*,*,#5325,.T.);
#7246=ORIENTED_EDGE('',*,*,#5322,.T.);
#7247=ORIENTED_EDGE('',*,*,#5319,.T.);
#7248=ORIENTED_EDGE('',*,*,#5316,.T.);
#7249=ORIENTED_EDGE('',*,*,#5312,.T.);
#7250=ORIENTED_EDGE('',*,*,#5409,.F.);
#7251=ORIENTED_EDGE('',*,*,#5410,.F.);
#7252=ORIENTED_EDGE('',*,*,#5365,.T.);
#7253=ORIENTED_EDGE('',*,*,#5362,.T.);
#7254=ORIENTED_EDGE('',*,*,#5359,.T.);
#7255=ORIENTED_EDGE('',*,*,#5356,.T.);
#7256=ORIENTED_EDGE('',*,*,#5353,.T.);
#7257=ORIENTED_EDGE('',*,*,#5350,.T.);
#7258=ORIENTED_EDGE('',*,*,#5347,.T.);
#7259=ORIENTED_EDGE('',*,*,#5344,.T.);
#7260=ORIENTED_EDGE('',*,*,#5340,.T.);
#7261=ORIENTED_EDGE('',*,*,#5414,.F.);
#7262=ORIENTED_EDGE('',*,*,#5415,.F.);
#7263=ORIENTED_EDGE('',*,*,#5393,.T.);
#7264=ORIENTED_EDGE('',*,*,#5390,.T.);
#7265=ORIENTED_EDGE('',*,*,#5387,.T.);
#7266=ORIENTED_EDGE('',*,*,#5384,.T.);
#7267=ORIENTED_EDGE('',*,*,#5381,.T.);
#7268=ORIENTED_EDGE('',*,*,#5378,.T.);
#7269=ORIENTED_EDGE('',*,*,#5375,.T.);
#7270=ORIENTED_EDGE('',*,*,#5372,.T.);
#7271=ORIENTED_EDGE('',*,*,#5368,.T.);
#7272=ORIENTED_EDGE('',*,*,#5418,.F.);
#7273=ORIENTED_EDGE('',*,*,#5399,.F.);
#7274=ORIENTED_EDGE('',*,*,#5309,.T.);
#7275=ORIENTED_EDGE('',*,*,#5306,.T.);
#7276=ORIENTED_EDGE('',*,*,#5303,.T.);
#7277=ORIENTED_EDGE('',*,*,#5300,.T.);
#7278=ORIENTED_EDGE('',*,*,#5297,.T.);
#7279=ORIENTED_EDGE('',*,*,#5294,.T.);
#7280=ORIENTED_EDGE('',*,*,#5291,.T.);
#7281=ORIENTED_EDGE('',*,*,#5288,.T.);
#7282=ORIENTED_EDGE('',*,*,#5396,.T.);
#7283=ORIENTED_EDGE('',*,*,#5419,.F.);
#7284=ORIENTED_EDGE('',*,*,#5420,.F.);
#7285=ORIENTED_EDGE('',*,*,#5421,.F.);
#7286=ORIENTED_EDGE('',*,*,#5422,.F.);
#7287=ORIENTED_EDGE('',*,*,#5421,.T.);
#7288=ORIENTED_EDGE('',*,*,#5423,.T.);
#7289=ORIENTED_EDGE('',*,*,#5424,.F.);
#7290=ORIENTED_EDGE('',*,*,#5425,.F.);
#7291=ORIENTED_EDGE('',*,*,#5426,.T.);
#7292=ORIENTED_EDGE('',*,*,#5427,.T.);
#7293=ORIENTED_EDGE('',*,*,#5428,.T.);
#7294=ORIENTED_EDGE('',*,*,#5424,.T.);
#7295=ORIENTED_EDGE('',*,*,#5429,.T.);
#7296=ORIENTED_EDGE('',*,*,#5426,.F.);
#7297=ORIENTED_EDGE('',*,*,#5423,.F.);
#7298=ORIENTED_EDGE('',*,*,#5420,.T.);
#7299=ORIENTED_EDGE('',*,*,#5430,.F.);
#7300=ORIENTED_EDGE('',*,*,#5431,.F.);
#7301=ORIENTED_EDGE('',*,*,#5432,.T.);
#7302=ORIENTED_EDGE('',*,*,#5433,.F.);
#7303=ORIENTED_EDGE('',*,*,#5434,.T.);
#7304=ORIENTED_EDGE('',*,*,#5435,.T.);
#7305=ORIENTED_EDGE('',*,*,#5436,.T.);
#7306=ORIENTED_EDGE('',*,*,#5437,.T.);
#7307=ORIENTED_EDGE('',*,*,#5438,.T.);
#7308=ORIENTED_EDGE('',*,*,#5427,.F.);
#7309=ORIENTED_EDGE('',*,*,#5436,.F.);
#7310=ORIENTED_EDGE('',*,*,#5439,.F.);
#7311=ORIENTED_EDGE('',*,*,#5440,.F.);
#7312=ORIENTED_EDGE('',*,*,#5437,.F.);
#7313=ORIENTED_EDGE('',*,*,#5435,.F.);
#7314=ORIENTED_EDGE('',*,*,#5428,.F.);
#7315=ORIENTED_EDGE('',*,*,#5438,.F.);
#7316=ORIENTED_EDGE('',*,*,#5440,.T.);
#7317=ORIENTED_EDGE('',*,*,#5441,.F.);
#7318=ORIENTED_EDGE('',*,*,#5442,.F.);
#7319=ORIENTED_EDGE('',*,*,#5443,.T.);
#7320=ORIENTED_EDGE('',*,*,#5444,.F.);
#7321=ORIENTED_EDGE('',*,*,#5445,.T.);
#7322=ORIENTED_EDGE('',*,*,#5422,.T.);
#7323=ORIENTED_EDGE('',*,*,#5425,.T.);
#7324=ORIENTED_EDGE('',*,*,#5439,.T.);
#7325=ORIENTED_EDGE('',*,*,#5434,.F.);
#7326=ORIENTED_EDGE('',*,*,#5446,.F.);
#7327=ORIENTED_EDGE('',*,*,#5441,.T.);
#7328=ORIENTED_EDGE('',*,*,#5442,.T.);
#7329=ORIENTED_EDGE('',*,*,#5446,.T.);
#7330=ORIENTED_EDGE('',*,*,#5433,.T.);
#7331=ORIENTED_EDGE('',*,*,#5447,.T.);
#7332=ORIENTED_EDGE('',*,*,#5448,.T.);
#7333=ORIENTED_EDGE('',*,*,#5449,.T.);
#7334=ORIENTED_EDGE('',*,*,#5448,.F.);
#7335=ORIENTED_EDGE('',*,*,#5450,.F.);
#7336=ORIENTED_EDGE('',*,*,#5451,.T.);
#7337=ORIENTED_EDGE('',*,*,#5429,.F.);
#7338=ORIENTED_EDGE('',*,*,#5451,.F.);
#7339=ORIENTED_EDGE('',*,*,#5452,.F.);
#7340=ORIENTED_EDGE('',*,*,#5453,.F.);
#7341=ORIENTED_EDGE('',*,*,#5454,.F.);
#7342=ORIENTED_EDGE('',*,*,#5447,.F.);
#7343=ORIENTED_EDGE('',*,*,#5432,.F.);
#7344=ORIENTED_EDGE('',*,*,#5455,.F.);
#7345=ORIENTED_EDGE('',*,*,#5452,.T.);
#7346=ORIENTED_EDGE('',*,*,#5450,.T.);
#7347=ORIENTED_EDGE('',*,*,#5449,.F.);
#7348=ORIENTED_EDGE('',*,*,#5454,.T.);
#7349=ORIENTED_EDGE('',*,*,#5456,.F.);
#7350=ORIENTED_EDGE('',*,*,#5443,.F.);
#7351=ORIENTED_EDGE('',*,*,#5431,.T.);
#7352=ORIENTED_EDGE('',*,*,#5457,.T.);
#7353=ORIENTED_EDGE('',*,*,#5444,.T.);
#7354=ORIENTED_EDGE('',*,*,#5456,.T.);
#7355=ORIENTED_EDGE('',*,*,#5453,.T.);
#7356=ORIENTED_EDGE('',*,*,#5455,.T.);
#7357=ORIENTED_EDGE('',*,*,#5419,.T.);
#7358=ORIENTED_EDGE('',*,*,#5445,.F.);
#7359=ORIENTED_EDGE('',*,*,#5457,.F.);
#7360=ORIENTED_EDGE('',*,*,#5430,.T.);
#7361=ORIENTED_EDGE('',*,*,#5458,.T.);
#7362=ORIENTED_EDGE('',*,*,#5459,.T.);
#7363=ORIENTED_EDGE('',*,*,#5460,.T.);
#7364=ORIENTED_EDGE('',*,*,#5461,.F.);
#7365=ORIENTED_EDGE('',*,*,#5462,.T.);
#7366=ORIENTED_EDGE('',*,*,#5463,.T.);
#7367=ORIENTED_EDGE('',*,*,#5464,.T.);
#7368=ORIENTED_EDGE('',*,*,#5459,.F.);
#7369=ORIENTED_EDGE('',*,*,#5465,.T.);
#7370=ORIENTED_EDGE('',*,*,#5466,.T.);
#7371=ORIENTED_EDGE('',*,*,#5467,.T.);
#7372=ORIENTED_EDGE('',*,*,#5463,.F.);
#7373=ORIENTED_EDGE('',*,*,#5468,.T.);
#7374=ORIENTED_EDGE('',*,*,#5469,.T.);
#7375=ORIENTED_EDGE('',*,*,#5470,.T.);
#7376=ORIENTED_EDGE('',*,*,#5466,.F.);
#7377=ORIENTED_EDGE('',*,*,#5471,.T.);
#7378=ORIENTED_EDGE('',*,*,#5472,.T.);
#7379=ORIENTED_EDGE('',*,*,#5473,.T.);
#7380=ORIENTED_EDGE('',*,*,#5469,.F.);
#7381=ORIENTED_EDGE('',*,*,#5474,.T.);
#7382=ORIENTED_EDGE('',*,*,#5461,.T.);
#7383=ORIENTED_EDGE('',*,*,#5475,.T.);
#7384=ORIENTED_EDGE('',*,*,#5472,.F.);
#7385=ORIENTED_EDGE('',*,*,#5474,.F.);
#7386=ORIENTED_EDGE('',*,*,#5471,.F.);
#7387=ORIENTED_EDGE('',*,*,#5468,.F.);
#7388=ORIENTED_EDGE('',*,*,#5465,.F.);
#7389=ORIENTED_EDGE('',*,*,#5462,.F.);
#7390=ORIENTED_EDGE('',*,*,#5458,.F.);
#7391=ORIENTED_EDGE('',*,*,#5475,.F.);
#7392=ORIENTED_EDGE('',*,*,#5460,.F.);
#7393=ORIENTED_EDGE('',*,*,#5464,.F.);
#7394=ORIENTED_EDGE('',*,*,#5467,.F.);
#7395=ORIENTED_EDGE('',*,*,#5470,.F.);
#7396=ORIENTED_EDGE('',*,*,#5473,.F.);
#7397=ORIENTED_EDGE('',*,*,#5476,.F.);
#7398=ORIENTED_EDGE('',*,*,#5477,.F.);
#7399=ORIENTED_EDGE('',*,*,#5478,.F.);
#7400=ORIENTED_EDGE('',*,*,#5479,.T.);
#7401=ORIENTED_EDGE('',*,*,#5477,.T.);
#7402=ORIENTED_EDGE('',*,*,#5479,.F.);
#7403=ORIENTED_EDGE('',*,*,#5480,.F.);
#7404=ORIENTED_EDGE('',*,*,#5481,.T.);
#7405=ORIENTED_EDGE('',*,*,#5478,.T.);
#7406=ORIENTED_EDGE('',*,*,#5481,.F.);
#7407=ORIENTED_EDGE('',*,*,#5482,.F.);
#7408=ORIENTED_EDGE('',*,*,#5483,.T.);
#7409=ORIENTED_EDGE('',*,*,#5480,.T.);
#7410=ORIENTED_EDGE('',*,*,#5483,.F.);
#7411=ORIENTED_EDGE('',*,*,#5482,.T.);
#7412=ORIENTED_EDGE('',*,*,#5484,.F.);
#7413=ORIENTED_EDGE('',*,*,#5485,.F.);
#7414=ORIENTED_EDGE('',*,*,#5486,.T.);
#7415=ORIENTED_EDGE('',*,*,#5484,.T.);
#7416=ORIENTED_EDGE('',*,*,#5486,.F.);
#7417=ORIENTED_EDGE('',*,*,#5476,.T.);
#7418=ORIENTED_EDGE('',*,*,#5487,.T.);
#7419=ORIENTED_EDGE('',*,*,#5485,.T.);
#7420=ORIENTED_EDGE('',*,*,#5487,.F.);
#7421=ORIENTED_EDGE('',*,*,#5488,.T.);
#7422=ORIENTED_EDGE('',*,*,#5489,.T.);
#7423=ORIENTED_EDGE('',*,*,#5490,.T.);
#7424=ORIENTED_EDGE('',*,*,#5491,.F.);
#7425=ORIENTED_EDGE('',*,*,#5492,.T.);
#7426=ORIENTED_EDGE('',*,*,#5493,.T.);
#7427=ORIENTED_EDGE('',*,*,#5494,.T.);
#7428=ORIENTED_EDGE('',*,*,#5489,.F.);
#7429=ORIENTED_EDGE('',*,*,#5495,.T.);
#7430=ORIENTED_EDGE('',*,*,#5496,.T.);
#7431=ORIENTED_EDGE('',*,*,#5497,.T.);
#7432=ORIENTED_EDGE('',*,*,#5493,.F.);
#7433=ORIENTED_EDGE('',*,*,#5498,.T.);
#7434=ORIENTED_EDGE('',*,*,#5499,.T.);
#7435=ORIENTED_EDGE('',*,*,#5500,.T.);
#7436=ORIENTED_EDGE('',*,*,#5496,.F.);
#7437=ORIENTED_EDGE('',*,*,#5501,.T.);
#7438=ORIENTED_EDGE('',*,*,#5502,.T.);
#7439=ORIENTED_EDGE('',*,*,#5503,.T.);
#7440=ORIENTED_EDGE('',*,*,#5499,.F.);
#7441=ORIENTED_EDGE('',*,*,#5504,.T.);
#7442=ORIENTED_EDGE('',*,*,#5491,.T.);
#7443=ORIENTED_EDGE('',*,*,#5505,.T.);
#7444=ORIENTED_EDGE('',*,*,#5502,.F.);
#7445=ORIENTED_EDGE('',*,*,#5504,.F.);
#7446=ORIENTED_EDGE('',*,*,#5501,.F.);
#7447=ORIENTED_EDGE('',*,*,#5498,.F.);
#7448=ORIENTED_EDGE('',*,*,#5495,.F.);
#7449=ORIENTED_EDGE('',*,*,#5492,.F.);
#7450=ORIENTED_EDGE('',*,*,#5488,.F.);
#7451=ORIENTED_EDGE('',*,*,#5505,.F.);
#7452=ORIENTED_EDGE('',*,*,#5490,.F.);
#7453=ORIENTED_EDGE('',*,*,#5494,.F.);
#7454=ORIENTED_EDGE('',*,*,#5497,.F.);
#7455=ORIENTED_EDGE('',*,*,#5500,.F.);
#7456=ORIENTED_EDGE('',*,*,#5503,.F.);
#7457=ORIENTED_EDGE('',*,*,#5506,.F.);
#7458=ORIENTED_EDGE('',*,*,#5507,.F.);
#7459=ORIENTED_EDGE('',*,*,#5508,.F.);
#7460=ORIENTED_EDGE('',*,*,#5509,.T.);
#7461=ORIENTED_EDGE('',*,*,#5507,.T.);
#7462=ORIENTED_EDGE('',*,*,#5509,.F.);
#7463=ORIENTED_EDGE('',*,*,#5510,.F.);
#7464=ORIENTED_EDGE('',*,*,#5511,.T.);
#7465=ORIENTED_EDGE('',*,*,#5508,.T.);
#7466=ORIENTED_EDGE('',*,*,#5511,.F.);
#7467=ORIENTED_EDGE('',*,*,#5512,.F.);
#7468=ORIENTED_EDGE('',*,*,#5513,.T.);
#7469=ORIENTED_EDGE('',*,*,#5510,.T.);
#7470=ORIENTED_EDGE('',*,*,#5513,.F.);
#7471=ORIENTED_EDGE('',*,*,#5512,.T.);
#7472=ORIENTED_EDGE('',*,*,#5514,.F.);
#7473=ORIENTED_EDGE('',*,*,#5515,.F.);
#7474=ORIENTED_EDGE('',*,*,#5516,.T.);
#7475=ORIENTED_EDGE('',*,*,#5514,.T.);
#7476=ORIENTED_EDGE('',*,*,#5516,.F.);
#7477=ORIENTED_EDGE('',*,*,#5506,.T.);
#7478=ORIENTED_EDGE('',*,*,#5517,.T.);
#7479=ORIENTED_EDGE('',*,*,#5515,.T.);
#7480=ORIENTED_EDGE('',*,*,#5517,.F.);
#7481=ORIENTED_EDGE('',*,*,#5518,.F.);
#7482=ORIENTED_EDGE('',*,*,#5519,.T.);
#7483=ORIENTED_EDGE('',*,*,#5520,.F.);
#7484=ORIENTED_EDGE('',*,*,#5519,.F.);
#7485=ORIENTED_EDGE('',*,*,#5521,.F.);
#7486=ORIENTED_EDGE('',*,*,#5522,.T.);
#7487=ORIENTED_EDGE('',*,*,#5523,.F.);
#7488=ORIENTED_EDGE('',*,*,#5522,.F.);
#7489=ORIENTED_EDGE('',*,*,#5524,.F.);
#7490=ORIENTED_EDGE('',*,*,#5525,.T.);
#7491=ORIENTED_EDGE('',*,*,#5526,.F.);
#7492=ORIENTED_EDGE('',*,*,#5525,.F.);
#7493=ORIENTED_EDGE('',*,*,#5527,.F.);
#7494=ORIENTED_EDGE('',*,*,#5528,.T.);
#7495=ORIENTED_EDGE('',*,*,#5529,.F.);
#7496=ORIENTED_EDGE('',*,*,#5528,.F.);
#7497=ORIENTED_EDGE('',*,*,#5530,.F.);
#7498=ORIENTED_EDGE('',*,*,#5531,.T.);
#7499=ORIENTED_EDGE('',*,*,#5532,.F.);
#7500=ORIENTED_EDGE('',*,*,#5531,.F.);
#7501=ORIENTED_EDGE('',*,*,#5533,.F.);
#7502=ORIENTED_EDGE('',*,*,#5534,.T.);
#7503=ORIENTED_EDGE('',*,*,#5535,.F.);
#7504=ORIENTED_EDGE('',*,*,#5534,.F.);
#7505=ORIENTED_EDGE('',*,*,#5536,.T.);
#7506=ORIENTED_EDGE('',*,*,#5537,.T.);
#7507=ORIENTED_EDGE('',*,*,#5538,.F.);
#7508=ORIENTED_EDGE('',*,*,#5539,.F.);
#7509=ORIENTED_EDGE('',*,*,#5540,.T.);
#7510=ORIENTED_EDGE('',*,*,#5539,.T.);
#7511=ORIENTED_EDGE('',*,*,#5541,.F.);
#7512=ORIENTED_EDGE('',*,*,#5542,.F.);
#7513=ORIENTED_EDGE('',*,*,#5543,.T.);
#7514=ORIENTED_EDGE('',*,*,#5542,.T.);
#7515=ORIENTED_EDGE('',*,*,#5544,.F.);
#7516=ORIENTED_EDGE('',*,*,#5545,.F.);
#7517=ORIENTED_EDGE('',*,*,#5546,.T.);
#7518=ORIENTED_EDGE('',*,*,#5545,.T.);
#7519=ORIENTED_EDGE('',*,*,#5547,.F.);
#7520=ORIENTED_EDGE('',*,*,#5537,.F.);
#7521=ORIENTED_EDGE('',*,*,#5547,.T.);
#7522=ORIENTED_EDGE('',*,*,#5544,.T.);
#7523=ORIENTED_EDGE('',*,*,#5541,.T.);
#7524=ORIENTED_EDGE('',*,*,#5538,.T.);
#7525=ORIENTED_EDGE('',*,*,#5520,.T.);
#7526=ORIENTED_EDGE('',*,*,#5523,.T.);
#7527=ORIENTED_EDGE('',*,*,#5526,.T.);
#7528=ORIENTED_EDGE('',*,*,#5529,.T.);
#7529=ORIENTED_EDGE('',*,*,#5532,.T.);
#7530=ORIENTED_EDGE('',*,*,#5535,.T.);
#7531=ORIENTED_EDGE('',*,*,#5546,.F.);
#7532=ORIENTED_EDGE('',*,*,#5536,.F.);
#7533=ORIENTED_EDGE('',*,*,#5540,.F.);
#7534=ORIENTED_EDGE('',*,*,#5543,.F.);
#7535=ORIENTED_EDGE('',*,*,#5518,.T.);
#7536=ORIENTED_EDGE('',*,*,#5521,.T.);
#7537=ORIENTED_EDGE('',*,*,#5524,.T.);
#7538=ORIENTED_EDGE('',*,*,#5527,.T.);
#7539=ORIENTED_EDGE('',*,*,#5530,.T.);
#7540=ORIENTED_EDGE('',*,*,#5533,.T.);
#7541=ORIENTED_EDGE('',*,*,#5548,.F.);
#7542=ORIENTED_EDGE('',*,*,#5549,.T.);
#7543=ORIENTED_EDGE('',*,*,#5550,.F.);
#7544=ORIENTED_EDGE('',*,*,#5549,.F.);
#7545=ORIENTED_EDGE('',*,*,#5551,.T.);
#7546=ORIENTED_EDGE('',*,*,#5552,.T.);
#7547=ORIENTED_EDGE('',*,*,#5553,.F.);
#7548=ORIENTED_EDGE('',*,*,#5554,.F.);
#7549=ORIENTED_EDGE('',*,*,#5550,.T.);
#7550=ORIENTED_EDGE('',*,*,#5555,.T.);
#7551=ORIENTED_EDGE('',*,*,#5554,.T.);
#7552=ORIENTED_EDGE('',*,*,#5556,.F.);
#7553=ORIENTED_EDGE('',*,*,#5557,.F.);
#7554=ORIENTED_EDGE('',*,*,#5558,.T.);
#7555=ORIENTED_EDGE('',*,*,#5557,.T.);
#7556=ORIENTED_EDGE('',*,*,#5559,.F.);
#7557=ORIENTED_EDGE('',*,*,#5560,.F.);
#7558=ORIENTED_EDGE('',*,*,#5561,.T.);
#7559=ORIENTED_EDGE('',*,*,#5560,.T.);
#7560=ORIENTED_EDGE('',*,*,#5562,.F.);
#7561=ORIENTED_EDGE('',*,*,#5563,.F.);
#7562=ORIENTED_EDGE('',*,*,#5564,.T.);
#7563=ORIENTED_EDGE('',*,*,#5563,.T.);
#7564=ORIENTED_EDGE('',*,*,#5565,.F.);
#7565=ORIENTED_EDGE('',*,*,#5566,.F.);
#7566=ORIENTED_EDGE('',*,*,#5548,.T.);
#7567=ORIENTED_EDGE('',*,*,#5567,.T.);
#7568=ORIENTED_EDGE('',*,*,#5566,.T.);
#7569=ORIENTED_EDGE('',*,*,#5568,.F.);
#7570=ORIENTED_EDGE('',*,*,#5552,.F.);
#7571=ORIENTED_EDGE('',*,*,#5568,.T.);
#7572=ORIENTED_EDGE('',*,*,#5565,.T.);
#7573=ORIENTED_EDGE('',*,*,#5562,.T.);
#7574=ORIENTED_EDGE('',*,*,#5559,.T.);
#7575=ORIENTED_EDGE('',*,*,#5556,.T.);
#7576=ORIENTED_EDGE('',*,*,#5553,.T.);
#7577=ORIENTED_EDGE('',*,*,#5567,.F.);
#7578=ORIENTED_EDGE('',*,*,#5551,.F.);
#7579=ORIENTED_EDGE('',*,*,#5555,.F.);
#7580=ORIENTED_EDGE('',*,*,#5558,.F.);
#7581=ORIENTED_EDGE('',*,*,#5561,.F.);
#7582=ORIENTED_EDGE('',*,*,#5564,.F.);
#7583=ORIENTED_EDGE('',*,*,#5569,.F.);
#7584=ORIENTED_EDGE('',*,*,#5570,.T.);
#7585=ORIENTED_EDGE('',*,*,#5571,.T.);
#7586=ORIENTED_EDGE('',*,*,#5570,.F.);
#7587=ORIENTED_EDGE('',*,*,#5572,.F.);
#7588=ORIENTED_EDGE('',*,*,#5573,.T.);
#7589=ORIENTED_EDGE('',*,*,#5574,.T.);
#7590=ORIENTED_EDGE('',*,*,#5573,.F.);
#7591=ORIENTED_EDGE('',*,*,#5572,.T.);
#7592=ORIENTED_EDGE('',*,*,#5569,.T.);
#7593=ORIENTED_EDGE('',*,*,#5574,.F.);
#7594=ORIENTED_EDGE('',*,*,#5571,.F.);
#7595=ORIENTED_EDGE('',*,*,#5575,.F.);
#7596=ORIENTED_EDGE('',*,*,#5576,.T.);
#7597=ORIENTED_EDGE('',*,*,#5577,.F.);
#7598=ORIENTED_EDGE('',*,*,#5578,.F.);
#7599=ORIENTED_EDGE('',*,*,#5579,.T.);
#7600=ORIENTED_EDGE('',*,*,#5580,.F.);
#7601=ORIENTED_EDGE('',*,*,#5579,.F.);
#7602=ORIENTED_EDGE('',*,*,#5581,.F.);
#7603=ORIENTED_EDGE('',*,*,#5582,.F.);
#7604=ORIENTED_EDGE('',*,*,#5576,.F.);
#7605=ORIENTED_EDGE('',*,*,#5583,.F.);
#7606=ORIENTED_EDGE('',*,*,#5584,.T.);
#7607=ORIENTED_EDGE('',*,*,#5585,.F.);
#7608=ORIENTED_EDGE('',*,*,#5586,.F.);
#7609=ORIENTED_EDGE('',*,*,#5587,.T.);
#7610=ORIENTED_EDGE('',*,*,#5588,.F.);
#7611=ORIENTED_EDGE('',*,*,#5587,.F.);
#7612=ORIENTED_EDGE('',*,*,#5589,.F.);
#7613=ORIENTED_EDGE('',*,*,#5590,.F.);
#7614=ORIENTED_EDGE('',*,*,#5584,.F.);
#7615=ORIENTED_EDGE('',*,*,#5591,.F.);
#7616=ORIENTED_EDGE('',*,*,#5592,.T.);
#7617=ORIENTED_EDGE('',*,*,#5593,.F.);
#7618=ORIENTED_EDGE('',*,*,#5594,.F.);
#7619=ORIENTED_EDGE('',*,*,#5595,.T.);
#7620=ORIENTED_EDGE('',*,*,#5596,.F.);
#7621=ORIENTED_EDGE('',*,*,#5595,.F.);
#7622=ORIENTED_EDGE('',*,*,#5597,.F.);
#7623=ORIENTED_EDGE('',*,*,#5598,.F.);
#7624=ORIENTED_EDGE('',*,*,#5592,.F.);
#7625=ORIENTED_EDGE('',*,*,#5599,.F.);
#7626=ORIENTED_EDGE('',*,*,#5600,.T.);
#7627=ORIENTED_EDGE('',*,*,#5601,.F.);
#7628=ORIENTED_EDGE('',*,*,#5602,.F.);
#7629=ORIENTED_EDGE('',*,*,#5603,.T.);
#7630=ORIENTED_EDGE('',*,*,#5604,.F.);
#7631=ORIENTED_EDGE('',*,*,#5603,.F.);
#7632=ORIENTED_EDGE('',*,*,#5605,.F.);
#7633=ORIENTED_EDGE('',*,*,#5606,.F.);
#7634=ORIENTED_EDGE('',*,*,#5600,.F.);
#7635=ORIENTED_EDGE('',*,*,#5577,.T.);
#7636=ORIENTED_EDGE('',*,*,#5575,.T.);
#7637=ORIENTED_EDGE('',*,*,#5582,.T.);
#7638=ORIENTED_EDGE('',*,*,#5607,.T.);
#7639=ORIENTED_EDGE('',*,*,#5593,.T.);
#7640=ORIENTED_EDGE('',*,*,#5591,.T.);
#7641=ORIENTED_EDGE('',*,*,#5598,.T.);
#7642=ORIENTED_EDGE('',*,*,#5608,.T.);
#7643=ORIENTED_EDGE('',*,*,#5609,.F.);
#7644=ORIENTED_EDGE('',*,*,#5610,.T.);
#7645=ORIENTED_EDGE('',*,*,#5611,.F.);
#7646=ORIENTED_EDGE('',*,*,#5612,.T.);
#7647=ORIENTED_EDGE('',*,*,#5585,.T.);
#7648=ORIENTED_EDGE('',*,*,#5583,.T.);
#7649=ORIENTED_EDGE('',*,*,#5590,.T.);
#7650=ORIENTED_EDGE('',*,*,#5613,.T.);
#7651=ORIENTED_EDGE('',*,*,#5601,.T.);
#7652=ORIENTED_EDGE('',*,*,#5599,.T.);
#7653=ORIENTED_EDGE('',*,*,#5606,.T.);
#7654=ORIENTED_EDGE('',*,*,#5614,.T.);
#7655=ORIENTED_EDGE('',*,*,#5615,.F.);
#7656=ORIENTED_EDGE('',*,*,#5616,.F.);
#7657=ORIENTED_EDGE('',*,*,#5617,.F.);
#7658=ORIENTED_EDGE('',*,*,#5618,.T.);
#7659=ORIENTED_EDGE('',*,*,#5609,.T.);
#7660=ORIENTED_EDGE('',*,*,#5619,.T.);
#7661=ORIENTED_EDGE('',*,*,#5620,.T.);
#7662=ORIENTED_EDGE('',*,*,#5621,.T.);
#7663=ORIENTED_EDGE('',*,*,#5622,.T.);
#7664=ORIENTED_EDGE('',*,*,#5623,.T.);
#7665=ORIENTED_EDGE('',*,*,#5617,.T.);
#7666=ORIENTED_EDGE('',*,*,#5624,.T.);
#7667=ORIENTED_EDGE('',*,*,#5625,.T.);
#7668=ORIENTED_EDGE('',*,*,#5626,.T.);
#7669=ORIENTED_EDGE('',*,*,#5627,.T.);
#7670=ORIENTED_EDGE('',*,*,#5628,.T.);
#7671=ORIENTED_EDGE('',*,*,#5581,.T.);
#7672=ORIENTED_EDGE('',*,*,#5578,.T.);
#7673=ORIENTED_EDGE('',*,*,#5612,.F.);
#7674=ORIENTED_EDGE('',*,*,#5629,.F.);
#7675=ORIENTED_EDGE('',*,*,#5630,.F.);
#7676=ORIENTED_EDGE('',*,*,#5619,.F.);
#7677=ORIENTED_EDGE('',*,*,#5608,.F.);
#7678=ORIENTED_EDGE('',*,*,#5597,.T.);
#7679=ORIENTED_EDGE('',*,*,#5594,.T.);
#7680=ORIENTED_EDGE('',*,*,#5607,.F.);
#7681=ORIENTED_EDGE('',*,*,#5630,.T.);
#7682=ORIENTED_EDGE('',*,*,#5631,.F.);
#7683=ORIENTED_EDGE('',*,*,#5632,.F.);
#7684=ORIENTED_EDGE('',*,*,#5620,.F.);
#7685=ORIENTED_EDGE('',*,*,#5632,.T.);
#7686=ORIENTED_EDGE('',*,*,#5633,.F.);
#7687=ORIENTED_EDGE('',*,*,#5634,.F.);
#7688=ORIENTED_EDGE('',*,*,#5621,.F.);
#7689=ORIENTED_EDGE('',*,*,#5580,.T.);
#7690=ORIENTED_EDGE('',*,*,#5588,.T.);
#7691=ORIENTED_EDGE('',*,*,#5596,.T.);
#7692=ORIENTED_EDGE('',*,*,#5604,.T.);
#7693=ORIENTED_EDGE('',*,*,#5634,.T.);
#7694=ORIENTED_EDGE('',*,*,#5635,.F.);
#7695=ORIENTED_EDGE('',*,*,#5636,.F.);
#7696=ORIENTED_EDGE('',*,*,#5622,.F.);
#7697=ORIENTED_EDGE('',*,*,#5589,.T.);
#7698=ORIENTED_EDGE('',*,*,#5586,.T.);
#7699=ORIENTED_EDGE('',*,*,#5618,.F.);
#7700=ORIENTED_EDGE('',*,*,#5623,.F.);
#7701=ORIENTED_EDGE('',*,*,#5636,.T.);
#7702=ORIENTED_EDGE('',*,*,#5637,.F.);
#7703=ORIENTED_EDGE('',*,*,#5614,.F.);
#7704=ORIENTED_EDGE('',*,*,#5605,.T.);
#7705=ORIENTED_EDGE('',*,*,#5602,.T.);
#7706=ORIENTED_EDGE('',*,*,#5613,.F.);
#7707=ORIENTED_EDGE('',*,*,#5616,.T.);
#7708=ORIENTED_EDGE('',*,*,#5638,.F.);
#7709=ORIENTED_EDGE('',*,*,#5639,.F.);
#7710=ORIENTED_EDGE('',*,*,#5624,.F.);
#7711=ORIENTED_EDGE('',*,*,#5639,.T.);
#7712=ORIENTED_EDGE('',*,*,#5640,.F.);
#7713=ORIENTED_EDGE('',*,*,#5641,.F.);
#7714=ORIENTED_EDGE('',*,*,#5625,.F.);
#7715=ORIENTED_EDGE('',*,*,#5641,.T.);
#7716=ORIENTED_EDGE('',*,*,#5642,.F.);
#7717=ORIENTED_EDGE('',*,*,#5643,.F.);
#7718=ORIENTED_EDGE('',*,*,#5626,.F.);
#7719=ORIENTED_EDGE('',*,*,#5643,.T.);
#7720=ORIENTED_EDGE('',*,*,#5644,.F.);
#7721=ORIENTED_EDGE('',*,*,#5645,.F.);
#7722=ORIENTED_EDGE('',*,*,#5627,.F.);
#7723=ORIENTED_EDGE('',*,*,#5645,.T.);
#7724=ORIENTED_EDGE('',*,*,#5646,.F.);
#7725=ORIENTED_EDGE('',*,*,#5610,.F.);
#7726=ORIENTED_EDGE('',*,*,#5628,.F.);
#7727=ORIENTED_EDGE('',*,*,#5611,.T.);
#7728=ORIENTED_EDGE('',*,*,#5646,.T.);
#7729=ORIENTED_EDGE('',*,*,#5644,.T.);
#7730=ORIENTED_EDGE('',*,*,#5642,.T.);
#7731=ORIENTED_EDGE('',*,*,#5640,.T.);
#7732=ORIENTED_EDGE('',*,*,#5638,.T.);
#7733=ORIENTED_EDGE('',*,*,#5615,.T.);
#7734=ORIENTED_EDGE('',*,*,#5637,.T.);
#7735=ORIENTED_EDGE('',*,*,#5635,.T.);
#7736=ORIENTED_EDGE('',*,*,#5633,.T.);
#7737=ORIENTED_EDGE('',*,*,#5631,.T.);
#7738=ORIENTED_EDGE('',*,*,#5629,.T.);
#7739=ORIENTED_EDGE('',*,*,#5647,.T.);
#7740=ORIENTED_EDGE('',*,*,#5648,.T.);
#7741=ORIENTED_EDGE('',*,*,#5649,.F.);
#7742=ORIENTED_EDGE('',*,*,#5650,.F.);
#7743=ORIENTED_EDGE('',*,*,#5651,.T.);
#7744=ORIENTED_EDGE('',*,*,#5650,.T.);
#7745=ORIENTED_EDGE('',*,*,#5652,.F.);
#7746=ORIENTED_EDGE('',*,*,#5653,.F.);
#7747=ORIENTED_EDGE('',*,*,#5654,.T.);
#7748=ORIENTED_EDGE('',*,*,#5653,.T.);
#7749=ORIENTED_EDGE('',*,*,#5655,.F.);
#7750=ORIENTED_EDGE('',*,*,#5656,.F.);
#7751=ORIENTED_EDGE('',*,*,#5657,.T.);
#7752=ORIENTED_EDGE('',*,*,#5656,.T.);
#7753=ORIENTED_EDGE('',*,*,#5658,.F.);
#7754=ORIENTED_EDGE('',*,*,#5659,.F.);
#7755=ORIENTED_EDGE('',*,*,#5660,.T.);
#7756=ORIENTED_EDGE('',*,*,#5659,.T.);
#7757=ORIENTED_EDGE('',*,*,#5661,.F.);
#7758=ORIENTED_EDGE('',*,*,#5662,.F.);
#7759=ORIENTED_EDGE('',*,*,#5663,.T.);
#7760=ORIENTED_EDGE('',*,*,#5662,.T.);
#7761=ORIENTED_EDGE('',*,*,#5664,.F.);
#7762=ORIENTED_EDGE('',*,*,#5665,.F.);
#7763=ORIENTED_EDGE('',*,*,#5666,.T.);
#7764=ORIENTED_EDGE('',*,*,#5665,.T.);
#7765=ORIENTED_EDGE('',*,*,#5667,.F.);
#7766=ORIENTED_EDGE('',*,*,#5668,.F.);
#7767=ORIENTED_EDGE('',*,*,#5669,.T.);
#7768=ORIENTED_EDGE('',*,*,#5668,.T.);
#7769=ORIENTED_EDGE('',*,*,#5670,.F.);
#7770=ORIENTED_EDGE('',*,*,#5648,.F.);
#7771=ORIENTED_EDGE('',*,*,#5670,.T.);
#7772=ORIENTED_EDGE('',*,*,#5667,.T.);
#7773=ORIENTED_EDGE('',*,*,#5664,.T.);
#7774=ORIENTED_EDGE('',*,*,#5661,.T.);
#7775=ORIENTED_EDGE('',*,*,#5658,.T.);
#7776=ORIENTED_EDGE('',*,*,#5655,.T.);
#7777=ORIENTED_EDGE('',*,*,#5652,.T.);
#7778=ORIENTED_EDGE('',*,*,#5649,.T.);
#7779=ORIENTED_EDGE('',*,*,#5669,.F.);
#7780=ORIENTED_EDGE('',*,*,#5647,.F.);
#7781=ORIENTED_EDGE('',*,*,#5651,.F.);
#7782=ORIENTED_EDGE('',*,*,#5654,.F.);
#7783=ORIENTED_EDGE('',*,*,#5657,.F.);
#7784=ORIENTED_EDGE('',*,*,#5660,.F.);
#7785=ORIENTED_EDGE('',*,*,#5663,.F.);
#7786=ORIENTED_EDGE('',*,*,#5666,.F.);
#7787=ORIENTED_EDGE('',*,*,#5671,.F.);
#7788=ORIENTED_EDGE('',*,*,#5672,.T.);
#7789=ORIENTED_EDGE('',*,*,#5673,.F.);
#7790=ORIENTED_EDGE('',*,*,#5674,.F.);
#7791=ORIENTED_EDGE('',*,*,#5675,.F.);
#7792=ORIENTED_EDGE('',*,*,#5674,.T.);
#7793=ORIENTED_EDGE('',*,*,#5676,.F.);
#7794=ORIENTED_EDGE('',*,*,#5677,.F.);
#7795=ORIENTED_EDGE('',*,*,#5678,.F.);
#7796=ORIENTED_EDGE('',*,*,#5677,.T.);
#7797=ORIENTED_EDGE('',*,*,#5679,.F.);
#7798=ORIENTED_EDGE('',*,*,#5680,.F.);
#7799=ORIENTED_EDGE('',*,*,#5681,.F.);
#7800=ORIENTED_EDGE('',*,*,#5680,.T.);
#7801=ORIENTED_EDGE('',*,*,#5682,.F.);
#7802=ORIENTED_EDGE('',*,*,#5683,.F.);
#7803=ORIENTED_EDGE('',*,*,#5684,.F.);
#7804=ORIENTED_EDGE('',*,*,#5683,.T.);
#7805=ORIENTED_EDGE('',*,*,#5685,.F.);
#7806=ORIENTED_EDGE('',*,*,#5686,.F.);
#7807=ORIENTED_EDGE('',*,*,#5687,.F.);
#7808=ORIENTED_EDGE('',*,*,#5686,.T.);
#7809=ORIENTED_EDGE('',*,*,#5688,.F.);
#7810=ORIENTED_EDGE('',*,*,#5689,.F.);
#7811=ORIENTED_EDGE('',*,*,#5690,.F.);
#7812=ORIENTED_EDGE('',*,*,#5689,.T.);
#7813=ORIENTED_EDGE('',*,*,#5691,.F.);
#7814=ORIENTED_EDGE('',*,*,#5692,.F.);
#7815=ORIENTED_EDGE('',*,*,#5693,.F.);
#7816=ORIENTED_EDGE('',*,*,#5692,.T.);
#7817=ORIENTED_EDGE('',*,*,#5694,.F.);
#7818=ORIENTED_EDGE('',*,*,#5672,.F.);
#7819=ORIENTED_EDGE('',*,*,#5693,.T.);
#7820=ORIENTED_EDGE('',*,*,#5671,.T.);
#7821=ORIENTED_EDGE('',*,*,#5675,.T.);
#7822=ORIENTED_EDGE('',*,*,#5678,.T.);
#7823=ORIENTED_EDGE('',*,*,#5681,.T.);
#7824=ORIENTED_EDGE('',*,*,#5684,.T.);
#7825=ORIENTED_EDGE('',*,*,#5687,.T.);
#7826=ORIENTED_EDGE('',*,*,#5690,.T.);
#7827=ORIENTED_EDGE('',*,*,#5694,.T.);
#7828=ORIENTED_EDGE('',*,*,#5691,.T.);
#7829=ORIENTED_EDGE('',*,*,#5688,.T.);
#7830=ORIENTED_EDGE('',*,*,#5685,.T.);
#7831=ORIENTED_EDGE('',*,*,#5682,.T.);
#7832=ORIENTED_EDGE('',*,*,#5679,.T.);
#7833=ORIENTED_EDGE('',*,*,#5676,.T.);
#7834=ORIENTED_EDGE('',*,*,#5673,.T.);
#7835=ORIENTED_EDGE('',*,*,#5695,.T.);
#7836=ORIENTED_EDGE('',*,*,#5696,.T.);
#7837=ORIENTED_EDGE('',*,*,#5697,.T.);
#7838=ORIENTED_EDGE('',*,*,#5696,.F.);
#7839=ORIENTED_EDGE('',*,*,#5697,.F.);
#7840=ORIENTED_EDGE('',*,*,#5698,.T.);
#7841=ORIENTED_EDGE('',*,*,#5699,.T.);
#7842=ORIENTED_EDGE('',*,*,#5698,.F.);
#7843=ORIENTED_EDGE('',*,*,#5700,.T.);
#7844=ORIENTED_EDGE('',*,*,#5695,.F.);
#7845=ORIENTED_EDGE('',*,*,#5700,.F.);
#7846=ORIENTED_EDGE('',*,*,#5701,.T.);
#7847=ORIENTED_EDGE('',*,*,#5702,.T.);
#7848=ORIENTED_EDGE('',*,*,#5701,.F.);
#7849=ORIENTED_EDGE('',*,*,#5702,.F.);
#7850=ORIENTED_EDGE('',*,*,#5699,.F.);
#7851=ORIENTED_EDGE('',*,*,#5703,.F.);
#7852=ORIENTED_EDGE('',*,*,#5704,.F.);
#7853=ORIENTED_EDGE('',*,*,#5705,.T.);
#7854=ORIENTED_EDGE('',*,*,#5703,.T.);
#7855=ORIENTED_EDGE('',*,*,#5705,.F.);
#7856=ORIENTED_EDGE('',*,*,#5706,.F.);
#7857=ORIENTED_EDGE('',*,*,#5707,.T.);
#7858=ORIENTED_EDGE('',*,*,#5704,.T.);
#7859=ORIENTED_EDGE('',*,*,#5707,.F.);
#7860=ORIENTED_EDGE('',*,*,#5708,.F.);
#7861=ORIENTED_EDGE('',*,*,#5709,.T.);
#7862=ORIENTED_EDGE('',*,*,#5706,.T.);
#7863=ORIENTED_EDGE('',*,*,#5709,.F.);
#7864=ORIENTED_EDGE('',*,*,#5708,.T.);
#7865=ORIENTED_EDGE('',*,*,#5710,.F.);
#7866=ORIENTED_EDGE('',*,*,#5711,.F.);
#7867=ORIENTED_EDGE('',*,*,#5712,.T.);
#7868=ORIENTED_EDGE('',*,*,#5710,.T.);
#7869=ORIENTED_EDGE('',*,*,#5712,.F.);
#7870=ORIENTED_EDGE('',*,*,#5713,.F.);
#7871=ORIENTED_EDGE('',*,*,#5714,.T.);
#7872=ORIENTED_EDGE('',*,*,#5711,.T.);
#7873=ORIENTED_EDGE('',*,*,#5714,.F.);
#7874=ORIENTED_EDGE('',*,*,#5715,.F.);
#7875=ORIENTED_EDGE('',*,*,#5716,.T.);
#7876=ORIENTED_EDGE('',*,*,#5713,.T.);
#7877=ORIENTED_EDGE('',*,*,#5716,.F.);
#7878=ORIENTED_EDGE('',*,*,#5715,.T.);
#7879=ORIENTED_EDGE('',*,*,#5717,.T.);
#7880=ORIENTED_EDGE('',*,*,#5718,.T.);
#7881=ORIENTED_EDGE('',*,*,#5719,.T.);
#7882=ORIENTED_EDGE('',*,*,#5720,.F.);
#7883=ORIENTED_EDGE('',*,*,#5721,.T.);
#7884=ORIENTED_EDGE('',*,*,#5722,.T.);
#7885=ORIENTED_EDGE('',*,*,#5723,.T.);
#7886=ORIENTED_EDGE('',*,*,#5718,.F.);
#7887=ORIENTED_EDGE('',*,*,#5724,.T.);
#7888=ORIENTED_EDGE('',*,*,#5725,.T.);
#7889=ORIENTED_EDGE('',*,*,#5726,.T.);
#7890=ORIENTED_EDGE('',*,*,#5722,.F.);
#7891=ORIENTED_EDGE('',*,*,#5727,.T.);
#7892=ORIENTED_EDGE('',*,*,#5728,.T.);
#7893=ORIENTED_EDGE('',*,*,#5729,.T.);
#7894=ORIENTED_EDGE('',*,*,#5725,.F.);
#7895=ORIENTED_EDGE('',*,*,#5730,.T.);
#7896=ORIENTED_EDGE('',*,*,#5731,.T.);
#7897=ORIENTED_EDGE('',*,*,#5732,.T.);
#7898=ORIENTED_EDGE('',*,*,#5728,.F.);
#7899=ORIENTED_EDGE('',*,*,#5733,.T.);
#7900=ORIENTED_EDGE('',*,*,#5720,.T.);
#7901=ORIENTED_EDGE('',*,*,#5734,.T.);
#7902=ORIENTED_EDGE('',*,*,#5731,.F.);
#7903=ORIENTED_EDGE('',*,*,#5733,.F.);
#7904=ORIENTED_EDGE('',*,*,#5730,.F.);
#7905=ORIENTED_EDGE('',*,*,#5727,.F.);
#7906=ORIENTED_EDGE('',*,*,#5724,.F.);
#7907=ORIENTED_EDGE('',*,*,#5721,.F.);
#7908=ORIENTED_EDGE('',*,*,#5717,.F.);
#7909=ORIENTED_EDGE('',*,*,#5734,.F.);
#7910=ORIENTED_EDGE('',*,*,#5719,.F.);
#7911=ORIENTED_EDGE('',*,*,#5723,.F.);
#7912=ORIENTED_EDGE('',*,*,#5726,.F.);
#7913=ORIENTED_EDGE('',*,*,#5729,.F.);
#7914=ORIENTED_EDGE('',*,*,#5732,.F.);
#7915=ORIENTED_EDGE('',*,*,#5735,.T.);
#7916=ORIENTED_EDGE('',*,*,#5736,.T.);
#7917=ORIENTED_EDGE('',*,*,#5737,.T.);
#7918=ORIENTED_EDGE('',*,*,#5736,.F.);
#7919=ORIENTED_EDGE('',*,*,#5737,.F.);
#7920=ORIENTED_EDGE('',*,*,#5738,.T.);
#7921=ORIENTED_EDGE('',*,*,#5739,.T.);
#7922=ORIENTED_EDGE('',*,*,#5738,.F.);
#7923=ORIENTED_EDGE('',*,*,#5740,.T.);
#7924=ORIENTED_EDGE('',*,*,#5735,.F.);
#7925=ORIENTED_EDGE('',*,*,#5740,.F.);
#7926=ORIENTED_EDGE('',*,*,#5741,.T.);
#7927=ORIENTED_EDGE('',*,*,#5742,.T.);
#7928=ORIENTED_EDGE('',*,*,#5741,.F.);
#7929=ORIENTED_EDGE('',*,*,#5742,.F.);
#7930=ORIENTED_EDGE('',*,*,#5739,.F.);
#7931=ORIENTED_EDGE('',*,*,#5743,.F.);
#7932=ORIENTED_EDGE('',*,*,#5744,.F.);
#7933=ORIENTED_EDGE('',*,*,#5745,.T.);
#7934=ORIENTED_EDGE('',*,*,#5743,.T.);
#7935=ORIENTED_EDGE('',*,*,#5745,.F.);
#7936=ORIENTED_EDGE('',*,*,#5746,.F.);
#7937=ORIENTED_EDGE('',*,*,#5747,.T.);
#7938=ORIENTED_EDGE('',*,*,#5744,.T.);
#7939=ORIENTED_EDGE('',*,*,#5747,.F.);
#7940=ORIENTED_EDGE('',*,*,#5748,.F.);
#7941=ORIENTED_EDGE('',*,*,#5749,.T.);
#7942=ORIENTED_EDGE('',*,*,#5746,.T.);
#7943=ORIENTED_EDGE('',*,*,#5749,.F.);
#7944=ORIENTED_EDGE('',*,*,#5748,.T.);
#7945=ORIENTED_EDGE('',*,*,#5750,.F.);
#7946=ORIENTED_EDGE('',*,*,#5751,.F.);
#7947=ORIENTED_EDGE('',*,*,#5752,.T.);
#7948=ORIENTED_EDGE('',*,*,#5750,.T.);
#7949=ORIENTED_EDGE('',*,*,#5752,.F.);
#7950=ORIENTED_EDGE('',*,*,#5753,.F.);
#7951=ORIENTED_EDGE('',*,*,#5754,.T.);
#7952=ORIENTED_EDGE('',*,*,#5751,.T.);
#7953=ORIENTED_EDGE('',*,*,#5754,.F.);
#7954=ORIENTED_EDGE('',*,*,#5755,.F.);
#7955=ORIENTED_EDGE('',*,*,#5756,.T.);
#7956=ORIENTED_EDGE('',*,*,#5753,.T.);
#7957=ORIENTED_EDGE('',*,*,#5756,.F.);
#7958=ORIENTED_EDGE('',*,*,#5755,.T.);
#7959=ORIENTED_EDGE('',*,*,#5757,.T.);
#7960=ORIENTED_EDGE('',*,*,#5758,.T.);
#7961=ORIENTED_EDGE('',*,*,#5759,.T.);
#7962=ORIENTED_EDGE('',*,*,#5760,.F.);
#7963=ORIENTED_EDGE('',*,*,#5761,.T.);
#7964=ORIENTED_EDGE('',*,*,#5762,.T.);
#7965=ORIENTED_EDGE('',*,*,#5763,.T.);
#7966=ORIENTED_EDGE('',*,*,#5758,.F.);
#7967=ORIENTED_EDGE('',*,*,#5764,.T.);
#7968=ORIENTED_EDGE('',*,*,#5765,.T.);
#7969=ORIENTED_EDGE('',*,*,#5766,.T.);
#7970=ORIENTED_EDGE('',*,*,#5762,.F.);
#7971=ORIENTED_EDGE('',*,*,#5767,.T.);
#7972=ORIENTED_EDGE('',*,*,#5768,.T.);
#7973=ORIENTED_EDGE('',*,*,#5769,.T.);
#7974=ORIENTED_EDGE('',*,*,#5765,.F.);
#7975=ORIENTED_EDGE('',*,*,#5770,.T.);
#7976=ORIENTED_EDGE('',*,*,#5771,.T.);
#7977=ORIENTED_EDGE('',*,*,#5772,.T.);
#7978=ORIENTED_EDGE('',*,*,#5768,.F.);
#7979=ORIENTED_EDGE('',*,*,#5773,.T.);
#7980=ORIENTED_EDGE('',*,*,#5760,.T.);
#7981=ORIENTED_EDGE('',*,*,#5774,.T.);
#7982=ORIENTED_EDGE('',*,*,#5771,.F.);
#7983=ORIENTED_EDGE('',*,*,#5773,.F.);
#7984=ORIENTED_EDGE('',*,*,#5770,.F.);
#7985=ORIENTED_EDGE('',*,*,#5767,.F.);
#7986=ORIENTED_EDGE('',*,*,#5764,.F.);
#7987=ORIENTED_EDGE('',*,*,#5761,.F.);
#7988=ORIENTED_EDGE('',*,*,#5757,.F.);
#7989=ORIENTED_EDGE('',*,*,#5774,.F.);
#7990=ORIENTED_EDGE('',*,*,#5759,.F.);
#7991=ORIENTED_EDGE('',*,*,#5763,.F.);
#7992=ORIENTED_EDGE('',*,*,#5766,.F.);
#7993=ORIENTED_EDGE('',*,*,#5769,.F.);
#7994=ORIENTED_EDGE('',*,*,#5772,.F.);
#7995=ORIENTED_EDGE('',*,*,#5775,.F.);
#7996=ORIENTED_EDGE('',*,*,#5776,.T.);
#7997=ORIENTED_EDGE('',*,*,#5777,.T.);
#7998=ORIENTED_EDGE('',*,*,#5776,.F.);
#7999=ORIENTED_EDGE('',*,*,#5778,.F.);
#8000=ORIENTED_EDGE('',*,*,#5779,.T.);
#8001=ORIENTED_EDGE('',*,*,#5780,.T.);
#8002=ORIENTED_EDGE('',*,*,#5779,.F.);
#8003=ORIENTED_EDGE('',*,*,#5778,.T.);
#8004=ORIENTED_EDGE('',*,*,#5775,.T.);
#8005=ORIENTED_EDGE('',*,*,#5780,.F.);
#8006=ORIENTED_EDGE('',*,*,#5777,.F.);
#8007=ORIENTED_EDGE('',*,*,#5781,.F.);
#8008=ORIENTED_EDGE('',*,*,#5782,.F.);
#8009=ORIENTED_EDGE('',*,*,#5783,.T.);
#8010=ORIENTED_EDGE('',*,*,#5781,.T.);
#8011=ORIENTED_EDGE('',*,*,#5783,.F.);
#8012=ORIENTED_EDGE('',*,*,#5784,.F.);
#8013=ORIENTED_EDGE('',*,*,#5785,.T.);
#8014=ORIENTED_EDGE('',*,*,#5782,.T.);
#8015=ORIENTED_EDGE('',*,*,#5785,.F.);
#8016=ORIENTED_EDGE('',*,*,#5786,.F.);
#8017=ORIENTED_EDGE('',*,*,#5787,.T.);
#8018=ORIENTED_EDGE('',*,*,#5784,.T.);
#8019=ORIENTED_EDGE('',*,*,#5787,.F.);
#8020=ORIENTED_EDGE('',*,*,#5786,.T.);
#8021=ORIENTED_EDGE('',*,*,#5788,.F.);
#8022=ORIENTED_EDGE('',*,*,#5789,.F.);
#8023=ORIENTED_EDGE('',*,*,#5790,.T.);
#8024=ORIENTED_EDGE('',*,*,#5788,.T.);
#8025=ORIENTED_EDGE('',*,*,#5790,.F.);
#8026=ORIENTED_EDGE('',*,*,#5791,.F.);
#8027=ORIENTED_EDGE('',*,*,#5792,.T.);
#8028=ORIENTED_EDGE('',*,*,#5789,.T.);
#8029=ORIENTED_EDGE('',*,*,#5792,.F.);
#8030=ORIENTED_EDGE('',*,*,#5793,.F.);
#8031=ORIENTED_EDGE('',*,*,#5794,.T.);
#8032=ORIENTED_EDGE('',*,*,#5791,.T.);
#8033=ORIENTED_EDGE('',*,*,#5794,.F.);
#8034=ORIENTED_EDGE('',*,*,#5793,.T.);
#8035=ORIENTED_EDGE('',*,*,#5795,.T.);
#8036=ORIENTED_EDGE('',*,*,#5796,.T.);
#8037=ORIENTED_EDGE('',*,*,#5797,.T.);
#8038=ORIENTED_EDGE('',*,*,#5798,.F.);
#8039=ORIENTED_EDGE('',*,*,#5799,.T.);
#8040=ORIENTED_EDGE('',*,*,#5800,.T.);
#8041=ORIENTED_EDGE('',*,*,#5801,.T.);
#8042=ORIENTED_EDGE('',*,*,#5796,.F.);
#8043=ORIENTED_EDGE('',*,*,#5802,.T.);
#8044=ORIENTED_EDGE('',*,*,#5803,.T.);
#8045=ORIENTED_EDGE('',*,*,#5804,.T.);
#8046=ORIENTED_EDGE('',*,*,#5800,.F.);
#8047=ORIENTED_EDGE('',*,*,#5805,.T.);
#8048=ORIENTED_EDGE('',*,*,#5806,.T.);
#8049=ORIENTED_EDGE('',*,*,#5807,.T.);
#8050=ORIENTED_EDGE('',*,*,#5803,.F.);
#8051=ORIENTED_EDGE('',*,*,#5808,.T.);
#8052=ORIENTED_EDGE('',*,*,#5809,.T.);
#8053=ORIENTED_EDGE('',*,*,#5810,.T.);
#8054=ORIENTED_EDGE('',*,*,#5806,.F.);
#8055=ORIENTED_EDGE('',*,*,#5811,.T.);
#8056=ORIENTED_EDGE('',*,*,#5798,.T.);
#8057=ORIENTED_EDGE('',*,*,#5812,.T.);
#8058=ORIENTED_EDGE('',*,*,#5809,.F.);
#8059=ORIENTED_EDGE('',*,*,#5811,.F.);
#8060=ORIENTED_EDGE('',*,*,#5808,.F.);
#8061=ORIENTED_EDGE('',*,*,#5805,.F.);
#8062=ORIENTED_EDGE('',*,*,#5802,.F.);
#8063=ORIENTED_EDGE('',*,*,#5799,.F.);
#8064=ORIENTED_EDGE('',*,*,#5795,.F.);
#8065=ORIENTED_EDGE('',*,*,#5812,.F.);
#8066=ORIENTED_EDGE('',*,*,#5797,.F.);
#8067=ORIENTED_EDGE('',*,*,#5801,.F.);
#8068=ORIENTED_EDGE('',*,*,#5804,.F.);
#8069=ORIENTED_EDGE('',*,*,#5807,.F.);
#8070=ORIENTED_EDGE('',*,*,#5810,.F.);
#8071=CYLINDRICAL_SURFACE('',#8922,0.165);
#8072=CYLINDRICAL_SURFACE('',#8925,0.164999999999999);
#8073=CYLINDRICAL_SURFACE('',#8928,0.210000000000001);
#8074=CYLINDRICAL_SURFACE('',#8931,0.21);
#8075=CYLINDRICAL_SURFACE('',#8934,0.21);
#8076=CYLINDRICAL_SURFACE('',#8937,0.210000000000001);
#8077=CYLINDRICAL_SURFACE('',#8940,0.274999999999999);
#8078=CYLINDRICAL_SURFACE('',#8943,0.275);
#8079=CYLINDRICAL_SURFACE('',#8946,0.275);
#8080=CYLINDRICAL_SURFACE('',#8949,0.274999999999999);
#8081=CYLINDRICAL_SURFACE('',#8952,0.164999999999999);
#8082=CYLINDRICAL_SURFACE('',#8955,0.164999999999999);
#8083=CYLINDRICAL_SURFACE('',#8958,0.165);
#8084=CYLINDRICAL_SURFACE('',#8961,0.164999999999999);
#8085=CYLINDRICAL_SURFACE('',#8971,0.475);
#8086=CYLINDRICAL_SURFACE('',#8976,0.475);
#8087=CYLINDRICAL_SURFACE('',#8981,0.275);
#8088=CYLINDRICAL_SURFACE('',#8983,0.275);
#8089=CYLINDRICAL_SURFACE('',#8999,0.475000000000001);
#8090=CYLINDRICAL_SURFACE('',#9004,0.475000000000001);
#8091=CYLINDRICAL_SURFACE('',#9009,0.274999999999999);
#8092=CYLINDRICAL_SURFACE('',#9011,0.274999999999999);
#8093=CYLINDRICAL_SURFACE('',#9146,0.225);
#8094=CYLINDRICAL_SURFACE('',#9148,0.225000000000001);
#8095=CYLINDRICAL_SURFACE('',#9184,0.375);
#8096=CYLINDRICAL_SURFACE('',#9189,0.375);
#8097=CYLINDRICAL_SURFACE('',#9194,0.375);
#8098=CYLINDRICAL_SURFACE('',#9199,0.375);
#8099=CYLINDRICAL_SURFACE('',#9204,0.225);
#8100=CYLINDRICAL_SURFACE('',#9206,0.225);
#8101=CYLINDRICAL_SURFACE('',#9208,0.225);
#8102=CYLINDRICAL_SURFACE('',#9210,0.225000000000001);
#8103=CYLINDRICAL_SURFACE('',#9263,0.21);
#8104=CYLINDRICAL_SURFACE('',#9288,0.2117);
#8105=CYLINDRICAL_SURFACE('',#9312,0.425);
#8106=CYLINDRICAL_SURFACE('',#9320,0.24505);
#8107=CYLINDRICAL_SURFACE('',#9336,0.35);
#8108=CYLINDRICAL_SURFACE('',#9344,0.1954);
#8109=CYLINDRICAL_SURFACE('',#9347,0.164999999999999);
#8110=CYLINDRICAL_SURFACE('',#9350,0.25);
#8111=CYLINDRICAL_SURFACE('',#9353,0.275);
#8112=CYLINDRICAL_SURFACE('',#9356,0.275);
#8113=CYLINDRICAL_SURFACE('',#9359,0.275);
#8114=CYLINDRICAL_SURFACE('',#9362,0.275);
#8115=CYLINDRICAL_SURFACE('',#9372,0.225);
#8116=CYLINDRICAL_SURFACE('',#9384,0.33);
#8117=CYLINDRICAL_SURFACE('',#9387,1.5);
#8118=CYLINDRICAL_SURFACE('',#9396,0.21);
#8119=CYLINDRICAL_SURFACE('',#9402,0.21);
#8120=CYLINDRICAL_SURFACE('',#9408,0.21);
#8121=CYLINDRICAL_SURFACE('',#9414,0.21);
#8122=CYLINDRICAL_SURFACE('',#9461,0.265);
#8123=CYLINDRICAL_SURFACE('',#9465,0.5);
#8124=CYLINDRICAL_SURFACE('',#9473,0.425);
#8125=CYLINDRICAL_SURFACE('',#9481,0.24505);
#8126=CYLINDRICAL_SURFACE('',#9498,0.215);
#8127=CYLINDRICAL_SURFACE('',#9502,0.45);
#8128=CYLINDRICAL_SURFACE('',#9510,0.35);
#8129=CYLINDRICAL_SURFACE('',#9518,0.1954);
#8130=CYLINDRICAL_SURFACE('',#9569,0.32);
#8131=CYLINDRICAL_SURFACE('',#9572,0.6);
#8132=CYLINDRICAL_SURFACE('',#9582,0.5);
#8133=CYLINDRICAL_SURFACE('',#9590,0.2942);
#8134=ADVANCED_FACE('',(#840),#8071,.F.);
#8135=ADVANCED_FACE('',(#841),#8072,.F.);
#8136=ADVANCED_FACE('',(#842),#8073,.F.);
#8137=ADVANCED_FACE('',(#843),#8074,.F.);
#8138=ADVANCED_FACE('',(#844),#8075,.F.);
#8139=ADVANCED_FACE('',(#845),#8076,.F.);
#8140=ADVANCED_FACE('',(#846),#8077,.F.);
#8141=ADVANCED_FACE('',(#847),#8078,.F.);
#8142=ADVANCED_FACE('',(#848),#8079,.F.);
#8143=ADVANCED_FACE('',(#849),#8080,.F.);
#8144=ADVANCED_FACE('',(#850),#8081,.F.);
#8145=ADVANCED_FACE('',(#851),#8082,.F.);
#8146=ADVANCED_FACE('',(#852),#8083,.F.);
#8147=ADVANCED_FACE('',(#853),#8084,.F.);
#8148=ADVANCED_FACE('',(#854),#468,.T.);
#8149=ADVANCED_FACE('',(#855),#469,.T.);
#8150=ADVANCED_FACE('',(#856),#470,.T.);
#8151=ADVANCED_FACE('',(#857),#471,.T.);
#8152=ADVANCED_FACE('',(#858,#378,#379,#380,#381,#382,#383,#384,#385,#386,
#387,#388,#389,#390,#391),#472,.T.);
#8153=ADVANCED_FACE('',(#859,#392,#393,#394,#395,#396,#397,#398,#399,#400,
#401,#402,#403,#404,#405),#473,.F.);
#8154=ADVANCED_FACE('',(#860),#8085,.F.);
#8155=ADVANCED_FACE('',(#861,#406),#474,.T.);
#8156=ADVANCED_FACE('',(#862),#8086,.F.);
#8157=ADVANCED_FACE('',(#863,#407),#475,.T.);
#8158=ADVANCED_FACE('',(#864),#8087,.F.);
#8159=ADVANCED_FACE('',(#865),#8088,.F.);
#8160=ADVANCED_FACE('',(#866),#476,.T.);
#8161=ADVANCED_FACE('',(#867),#477,.T.);
#8162=ADVANCED_FACE('',(#868),#478,.T.);
#8163=ADVANCED_FACE('',(#869),#479,.T.);
#8164=ADVANCED_FACE('',(#870,#408,#409),#480,.T.);
#8165=ADVANCED_FACE('',(#871,#410,#411),#481,.F.);
#8166=ADVANCED_FACE('',(#872),#482,.T.);
#8167=ADVANCED_FACE('',(#873),#483,.T.);
#8168=ADVANCED_FACE('',(#874),#484,.T.);
#8169=ADVANCED_FACE('',(#875),#485,.T.);
#8170=ADVANCED_FACE('',(#876),#486,.T.);
#8171=ADVANCED_FACE('',(#877),#487,.F.);
#8172=ADVANCED_FACE('',(#878),#8089,.F.);
#8173=ADVANCED_FACE('',(#879,#412),#488,.T.);
#8174=ADVANCED_FACE('',(#880),#8090,.F.);
#8175=ADVANCED_FACE('',(#881,#413),#489,.T.);
#8176=ADVANCED_FACE('',(#882),#8091,.F.);
#8177=ADVANCED_FACE('',(#883),#8092,.F.);
#8178=ADVANCED_FACE('',(#884),#490,.T.);
#8179=ADVANCED_FACE('',(#885),#491,.T.);
#8180=ADVANCED_FACE('',(#886),#492,.T.);
#8181=ADVANCED_FACE('',(#887),#493,.T.);
#8182=ADVANCED_FACE('',(#888,#414,#415),#494,.T.);
#8183=ADVANCED_FACE('',(#889,#416,#417),#495,.F.);
#8184=ADVANCED_FACE('',(#890),#496,.T.);
#8185=ADVANCED_FACE('',(#891),#497,.T.);
#8186=ADVANCED_FACE('',(#892),#498,.T.);
#8187=ADVANCED_FACE('',(#893),#499,.T.);
#8188=ADVANCED_FACE('',(#894),#500,.T.);
#8189=ADVANCED_FACE('',(#895),#501,.F.);
#8190=ADVANCED_FACE('',(#896),#502,.F.);
#8191=ADVANCED_FACE('',(#897),#503,.F.);
#8192=ADVANCED_FACE('',(#898),#504,.F.);
#8193=ADVANCED_FACE('',(#899),#505,.T.);
#8194=ADVANCED_FACE('',(#900),#506,.F.);
#8195=ADVANCED_FACE('',(#901),#507,.F.);
#8196=ADVANCED_FACE('',(#902),#508,.F.);
#8197=ADVANCED_FACE('',(#903),#509,.T.);
#8198=ADVANCED_FACE('',(#904),#510,.F.);
#8199=ADVANCED_FACE('',(#905),#511,.F.);
#8200=ADVANCED_FACE('',(#906),#512,.F.);
#8201=ADVANCED_FACE('',(#907),#513,.T.);
#8202=ADVANCED_FACE('',(#908),#514,.F.);
#8203=ADVANCED_FACE('',(#909),#515,.F.);
#8204=ADVANCED_FACE('',(#910),#516,.F.);
#8205=ADVANCED_FACE('',(#911),#517,.T.);
#8206=ADVANCED_FACE('',(#912),#518,.F.);
#8207=ADVANCED_FACE('',(#913),#519,.F.);
#8208=ADVANCED_FACE('',(#914),#520,.F.);
#8209=ADVANCED_FACE('',(#915),#521,.T.);
#8210=ADVANCED_FACE('',(#916),#522,.F.);
#8211=ADVANCED_FACE('',(#917),#523,.F.);
#8212=ADVANCED_FACE('',(#918),#524,.F.);
#8213=ADVANCED_FACE('',(#919),#525,.T.);
#8214=ADVANCED_FACE('',(#920),#526,.F.);
#8215=ADVANCED_FACE('',(#921),#527,.F.);
#8216=ADVANCED_FACE('',(#922),#528,.F.);
#8217=ADVANCED_FACE('',(#923),#529,.T.);
#8218=ADVANCED_FACE('',(#924),#530,.F.);
#8219=ADVANCED_FACE('',(#925),#531,.F.);
#8220=ADVANCED_FACE('',(#926),#532,.F.);
#8221=ADVANCED_FACE('',(#927),#533,.T.);
#8222=ADVANCED_FACE('',(#928),#534,.F.);
#8223=ADVANCED_FACE('',(#929),#535,.F.);
#8224=ADVANCED_FACE('',(#930),#536,.F.);
#8225=ADVANCED_FACE('',(#931),#537,.T.);
#8226=ADVANCED_FACE('',(#932),#538,.F.);
#8227=ADVANCED_FACE('',(#933),#539,.F.);
#8228=ADVANCED_FACE('',(#934),#540,.F.);
#8229=ADVANCED_FACE('',(#935),#541,.T.);
#8230=ADVANCED_FACE('',(#936),#542,.F.);
#8231=ADVANCED_FACE('',(#937),#543,.F.);
#8232=ADVANCED_FACE('',(#938),#544,.F.);
#8233=ADVANCED_FACE('',(#939),#545,.T.);
#8234=ADVANCED_FACE('',(#940),#546,.F.);
#8235=ADVANCED_FACE('',(#941),#547,.F.);
#8236=ADVANCED_FACE('',(#942),#548,.F.);
#8237=ADVANCED_FACE('',(#943),#549,.T.);
#8238=ADVANCED_FACE('',(#944),#550,.F.);
#8239=ADVANCED_FACE('',(#945),#551,.F.);
#8240=ADVANCED_FACE('',(#946),#552,.F.);
#8241=ADVANCED_FACE('',(#947),#553,.T.);
#8242=ADVANCED_FACE('',(#948),#554,.F.);
#8243=ADVANCED_FACE('',(#949),#555,.F.);
#8244=ADVANCED_FACE('',(#950),#556,.F.);
#8245=ADVANCED_FACE('',(#951),#557,.T.);
#8246=ADVANCED_FACE('',(#952),#558,.F.);
#8247=ADVANCED_FACE('',(#953),#559,.F.);
#8248=ADVANCED_FACE('',(#954),#560,.F.);
#8249=ADVANCED_FACE('',(#955),#561,.T.);
#8250=ADVANCED_FACE('',(#956),#562,.F.);
#8251=ADVANCED_FACE('',(#957),#563,.F.);
#8252=ADVANCED_FACE('',(#958),#564,.F.);
#8253=ADVANCED_FACE('',(#959),#565,.T.);
#8254=ADVANCED_FACE('',(#960),#566,.F.);
#8255=ADVANCED_FACE('',(#961),#567,.F.);
#8256=ADVANCED_FACE('',(#962),#568,.F.);
#8257=ADVANCED_FACE('',(#963),#569,.T.);
#8258=ADVANCED_FACE('',(#964),#570,.F.);
#8259=ADVANCED_FACE('',(#965),#571,.F.);
#8260=ADVANCED_FACE('',(#966),#572,.F.);
#8261=ADVANCED_FACE('',(#967),#573,.T.);
#8262=ADVANCED_FACE('',(#968),#574,.F.);
#8263=ADVANCED_FACE('',(#969),#575,.F.);
#8264=ADVANCED_FACE('',(#970),#576,.F.);
#8265=ADVANCED_FACE('',(#971),#577,.T.);
#8266=ADVANCED_FACE('',(#972),#578,.F.);
#8267=ADVANCED_FACE('',(#973),#579,.F.);
#8268=ADVANCED_FACE('',(#974),#580,.F.);
#8269=ADVANCED_FACE('',(#975),#581,.T.);
#8270=ADVANCED_FACE('',(#976),#582,.F.);
#8271=ADVANCED_FACE('',(#977),#583,.F.);
#8272=ADVANCED_FACE('',(#978),#584,.F.);
#8273=ADVANCED_FACE('',(#979),#585,.T.);
#8274=ADVANCED_FACE('',(#980),#586,.F.);
#8275=ADVANCED_FACE('',(#981),#587,.F.);
#8276=ADVANCED_FACE('',(#982),#588,.F.);
#8277=ADVANCED_FACE('',(#983),#589,.T.);
#8278=ADVANCED_FACE('',(#984),#590,.F.);
#8279=ADVANCED_FACE('',(#985),#591,.F.);
#8280=ADVANCED_FACE('',(#986),#592,.F.);
#8281=ADVANCED_FACE('',(#987),#593,.T.);
#8282=ADVANCED_FACE('',(#988),#594,.F.);
#8283=ADVANCED_FACE('',(#989),#595,.F.);
#8284=ADVANCED_FACE('',(#990),#596,.F.);
#8285=ADVANCED_FACE('',(#991),#597,.T.);
#8286=ADVANCED_FACE('',(#992),#598,.F.);
#8287=ADVANCED_FACE('',(#993),#599,.F.);
#8288=ADVANCED_FACE('',(#994),#600,.F.);
#8289=ADVANCED_FACE('',(#995),#601,.T.);
#8290=ADVANCED_FACE('',(#996),#602,.F.);
#8291=ADVANCED_FACE('',(#997),#603,.F.);
#8292=ADVANCED_FACE('',(#998),#604,.F.);
#8293=ADVANCED_FACE('',(#999),#605,.T.);
#8294=ADVANCED_FACE('',(#1000),#606,.F.);
#8295=ADVANCED_FACE('',(#1001),#607,.F.);
#8296=ADVANCED_FACE('',(#1002),#608,.F.);
#8297=ADVANCED_FACE('',(#1003),#609,.T.);
#8298=ADVANCED_FACE('',(#1004),#610,.F.);
#8299=ADVANCED_FACE('',(#1005),#611,.F.);
#8300=ADVANCED_FACE('',(#1006),#612,.F.);
#8301=ADVANCED_FACE('',(#1007),#613,.T.);
#8302=ADVANCED_FACE('',(#1008),#614,.F.);
#8303=ADVANCED_FACE('',(#1009),#615,.F.);
#8304=ADVANCED_FACE('',(#1010),#616,.F.);
#8305=ADVANCED_FACE('',(#1011),#617,.T.);
#8306=ADVANCED_FACE('',(#1012,#418,#419),#618,.T.);
#8307=ADVANCED_FACE('',(#1013),#8093,.F.);
#8308=ADVANCED_FACE('',(#1014),#8094,.F.);
#8309=ADVANCED_FACE('',(#1015),#619,.T.);
#8310=ADVANCED_FACE('',(#1016),#620,.T.);
#8311=ADVANCED_FACE('',(#1017),#621,.T.);
#8312=ADVANCED_FACE('',(#1018),#622,.T.);
#8313=ADVANCED_FACE('',(#1019,#420,#421),#623,.F.);
#8314=ADVANCED_FACE('',(#1020),#624,.T.);
#8315=ADVANCED_FACE('',(#1021),#625,.T.);
#8316=ADVANCED_FACE('',(#1022),#626,.T.);
#8317=ADVANCED_FACE('',(#1023),#627,.T.);
#8318=ADVANCED_FACE('',(#1024),#628,.T.);
#8319=ADVANCED_FACE('',(#1025),#629,.F.);
#8320=ADVANCED_FACE('',(#1026),#630,.T.);
#8321=ADVANCED_FACE('',(#1027),#631,.T.);
#8322=ADVANCED_FACE('',(#1028),#632,.T.);
#8323=ADVANCED_FACE('',(#1029),#633,.T.);
#8324=ADVANCED_FACE('',(#1030),#634,.T.);
#8325=ADVANCED_FACE('',(#1031),#635,.F.);
#8326=ADVANCED_FACE('',(#1032),#636,.T.);
#8327=ADVANCED_FACE('',(#1033),#637,.T.);
#8328=ADVANCED_FACE('',(#1034),#638,.T.);
#8329=ADVANCED_FACE('',(#1035),#639,.T.);
#8330=ADVANCED_FACE('',(#1036),#640,.T.);
#8331=ADVANCED_FACE('',(#1037),#641,.F.);
#8332=ADVANCED_FACE('',(#1038),#642,.T.);
#8333=ADVANCED_FACE('',(#1039),#643,.T.);
#8334=ADVANCED_FACE('',(#1040),#644,.T.);
#8335=ADVANCED_FACE('',(#1041),#645,.T.);
#8336=ADVANCED_FACE('',(#1042),#646,.T.);
#8337=ADVANCED_FACE('',(#1043),#647,.F.);
#8338=ADVANCED_FACE('',(#1044),#8095,.F.);
#8339=ADVANCED_FACE('',(#1045,#422),#648,.T.);
#8340=ADVANCED_FACE('',(#1046),#8096,.F.);
#8341=ADVANCED_FACE('',(#1047,#423),#649,.T.);
#8342=ADVANCED_FACE('',(#1048),#8097,.F.);
#8343=ADVANCED_FACE('',(#1049,#424),#650,.T.);
#8344=ADVANCED_FACE('',(#1050),#8098,.F.);
#8345=ADVANCED_FACE('',(#1051,#425),#651,.T.);
#8346=ADVANCED_FACE('',(#1052),#8099,.F.);
#8347=ADVANCED_FACE('',(#1053),#8100,.F.);
#8348=ADVANCED_FACE('',(#1054),#8101,.F.);
#8349=ADVANCED_FACE('',(#1055),#8102,.F.);
#8350=ADVANCED_FACE('',(#1056),#652,.T.);
#8351=ADVANCED_FACE('',(#1057),#653,.T.);
#8352=ADVANCED_FACE('',(#1058),#654,.T.);
#8353=ADVANCED_FACE('',(#1059),#655,.T.);
#8354=ADVANCED_FACE('',(#1060,#426,#427,#428,#429),#656,.T.);
#8355=ADVANCED_FACE('',(#1061),#657,.T.);
#8356=ADVANCED_FACE('',(#1062),#658,.T.);
#8357=ADVANCED_FACE('',(#1063),#659,.T.);
#8358=ADVANCED_FACE('',(#1064),#660,.T.);
#8359=ADVANCED_FACE('',(#1065),#661,.T.);
#8360=ADVANCED_FACE('',(#1066,#430,#431,#432,#433),#662,.T.);
#8361=ADVANCED_FACE('',(#1067),#663,.T.);
#8362=ADVANCED_FACE('',(#1068),#664,.T.);
#8363=ADVANCED_FACE('',(#1069),#665,.F.);
#8364=ADVANCED_FACE('',(#1070),#666,.F.);
#8365=ADVANCED_FACE('',(#1071),#667,.F.);
#8366=ADVANCED_FACE('',(#1072),#668,.F.);
#8367=ADVANCED_FACE('',(#1073),#669,.F.);
#8368=ADVANCED_FACE('',(#1074),#670,.F.);
#8369=ADVANCED_FACE('',(#1075),#671,.F.);
#8370=ADVANCED_FACE('',(#1076),#672,.F.);
#8371=ADVANCED_FACE('',(#1077),#673,.F.);
#8372=ADVANCED_FACE('',(#1078),#674,.F.);
#8373=ADVANCED_FACE('',(#1079),#675,.F.);
#8374=ADVANCED_FACE('',(#1080),#676,.F.);
#8375=ADVANCED_FACE('',(#1081),#677,.F.);
#8376=ADVANCED_FACE('',(#1082),#678,.F.);
#8377=ADVANCED_FACE('',(#1083),#679,.F.);
#8378=ADVANCED_FACE('',(#1084),#680,.F.);
#8379=ADVANCED_FACE('',(#1085),#681,.F.);
#8380=ADVANCED_FACE('',(#1086),#682,.F.);
#8381=ADVANCED_FACE('',(#1087),#683,.F.);
#8382=ADVANCED_FACE('',(#1088),#684,.F.);
#8383=ADVANCED_FACE('',(#1089),#685,.F.);
#8384=ADVANCED_FACE('',(#1090),#686,.F.);
#8385=ADVANCED_FACE('',(#1091),#687,.F.);
#8386=ADVANCED_FACE('',(#1092),#688,.F.);
#8387=ADVANCED_FACE('',(#1093),#689,.F.);
#8388=ADVANCED_FACE('',(#1094),#690,.F.);
#8389=ADVANCED_FACE('',(#1095),#691,.F.);
#8390=ADVANCED_FACE('',(#1096),#692,.F.);
#8391=ADVANCED_FACE('',(#1097),#693,.F.);
#8392=ADVANCED_FACE('',(#1098),#694,.F.);
#8393=ADVANCED_FACE('',(#1099),#695,.F.);
#8394=ADVANCED_FACE('',(#1100),#696,.F.);
#8395=ADVANCED_FACE('',(#1101),#697,.F.);
#8396=ADVANCED_FACE('',(#1102),#698,.F.);
#8397=ADVANCED_FACE('',(#1103),#699,.F.);
#8398=ADVANCED_FACE('',(#1104),#700,.F.);
#8399=ADVANCED_FACE('',(#1105),#701,.F.);
#8400=ADVANCED_FACE('',(#1106),#8103,.F.);
#8401=ADVANCED_FACE('',(#1107),#702,.T.);
#8402=ADVANCED_FACE('',(#1108),#703,.T.);
#8403=ADVANCED_FACE('',(#1109),#704,.T.);
#8404=ADVANCED_FACE('',(#1110),#705,.T.);
#8405=ADVANCED_FACE('',(#1111),#706,.T.);
#8406=ADVANCED_FACE('',(#1112),#707,.T.);
#8407=ADVANCED_FACE('',(#1113),#708,.T.);
#8408=ADVANCED_FACE('',(#1114),#709,.T.);
#8409=ADVANCED_FACE('',(#1115,#434),#710,.T.);
#8410=ADVANCED_FACE('',(#1116,#435),#711,.F.);
#8411=ADVANCED_FACE('',(#1117),#712,.F.);
#8412=ADVANCED_FACE('',(#1118),#713,.T.);
#8413=ADVANCED_FACE('',(#1119,#436),#714,.T.);
#8414=ADVANCED_FACE('',(#1120),#715,.T.);
#8415=ADVANCED_FACE('',(#1121),#716,.T.);
#8416=ADVANCED_FACE('',(#1122),#717,.F.);
#8417=ADVANCED_FACE('',(#1123),#718,.T.);
#8418=ADVANCED_FACE('',(#1124),#719,.T.);
#8419=ADVANCED_FACE('',(#1125),#720,.T.);
#8420=ADVANCED_FACE('',(#1126),#8104,.F.);
#8421=ADVANCED_FACE('',(#1127),#721,.F.);
#8422=ADVANCED_FACE('',(#1128),#722,.F.);
#8423=ADVANCED_FACE('',(#1129),#723,.T.);
#8424=ADVANCED_FACE('',(#1130),#724,.T.);
#8425=ADVANCED_FACE('',(#1131),#725,.F.);
#8426=ADVANCED_FACE('',(#1132),#726,.F.);
#8427=ADVANCED_FACE('',(#1133),#727,.F.);
#8428=ADVANCED_FACE('',(#1134),#728,.F.);
#8429=ADVANCED_FACE('',(#1135),#729,.F.);
#8430=ADVANCED_FACE('',(#1136),#730,.F.);
#8431=ADVANCED_FACE('',(#1137),#731,.F.);
#8432=ADVANCED_FACE('',(#1138),#732,.F.);
#8433=ADVANCED_FACE('',(#1139),#733,.F.);
#8434=ADVANCED_FACE('',(#1140),#734,.T.);
#8435=ADVANCED_FACE('',(#1141),#243,.T.);
#8436=ADVANCED_FACE('',(#1142),#8105,.T.);
#8437=ADVANCED_FACE('',(#1143),#244,.T.);
#8438=ADVANCED_FACE('',(#1144,#437),#735,.T.);
#8439=ADVANCED_FACE('',(#1145),#245,.T.);
#8440=ADVANCED_FACE('',(#1146),#8106,.T.);
#8441=ADVANCED_FACE('',(#1147),#736,.F.);
#8442=ADVANCED_FACE('',(#1148),#737,.F.);
#8443=ADVANCED_FACE('',(#1149),#738,.F.);
#8444=ADVANCED_FACE('',(#1150),#739,.F.);
#8445=ADVANCED_FACE('',(#1151),#740,.F.);
#8446=ADVANCED_FACE('',(#1152),#741,.F.);
#8447=ADVANCED_FACE('',(#1153),#742,.F.);
#8448=ADVANCED_FACE('',(#1154),#743,.F.);
#8449=ADVANCED_FACE('',(#1155),#744,.F.);
#8450=ADVANCED_FACE('',(#1156),#745,.T.);
#8451=ADVANCED_FACE('',(#1157),#246,.T.);
#8452=ADVANCED_FACE('',(#1158),#8107,.T.);
#8453=ADVANCED_FACE('',(#1159),#247,.T.);
#8454=ADVANCED_FACE('',(#1160,#438),#746,.T.);
#8455=ADVANCED_FACE('',(#1161),#248,.T.);
#8456=ADVANCED_FACE('',(#1162),#8108,.T.);
#8457=ADVANCED_FACE('',(#1163),#8109,.F.);
#8458=ADVANCED_FACE('',(#1164),#8110,.F.);
#8459=ADVANCED_FACE('',(#1165),#8111,.F.);
#8460=ADVANCED_FACE('',(#1166),#8112,.F.);
#8461=ADVANCED_FACE('',(#1167),#8113,.F.);
#8462=ADVANCED_FACE('',(#1168),#8114,.F.);
#8463=ADVANCED_FACE('',(#1169),#747,.T.);
#8464=ADVANCED_FACE('',(#1170),#748,.T.);
#8465=ADVANCED_FACE('',(#1171),#749,.T.);
#8466=ADVANCED_FACE('',(#1172),#750,.T.);
#8467=ADVANCED_FACE('',(#1173,#439,#440,#441,#442,#443,#444),#751,.T.);
#8468=ADVANCED_FACE('',(#1174,#445,#446,#447,#448,#449,#450),#752,.F.);
#8469=ADVANCED_FACE('',(#1175),#8115,.F.);
#8470=ADVANCED_FACE('',(#1176,#451),#753,.T.);
#8471=ADVANCED_FACE('',(#1177),#754,.T.);
#8472=ADVANCED_FACE('',(#1178),#755,.T.);
#8473=ADVANCED_FACE('',(#1179),#756,.T.);
#8474=ADVANCED_FACE('',(#1180,#452),#757,.T.);
#8475=ADVANCED_FACE('',(#1181),#758,.T.);
#8476=ADVANCED_FACE('',(#1182),#759,.T.);
#8477=ADVANCED_FACE('',(#1183),#760,.F.);
#8478=ADVANCED_FACE('',(#1184),#8116,.F.);
#8479=ADVANCED_FACE('',(#1185),#8117,.T.);
#8480=ADVANCED_FACE('',(#1186,#453),#761,.T.);
#8481=ADVANCED_FACE('',(#1187,#454),#762,.F.);
#8482=ADVANCED_FACE('',(#1188),#763,.T.);
#8483=ADVANCED_FACE('',(#1189),#8118,.F.);
#8484=ADVANCED_FACE('',(#1190),#764,.T.);
#8485=ADVANCED_FACE('',(#1191),#8119,.F.);
#8486=ADVANCED_FACE('',(#1192),#765,.T.);
#8487=ADVANCED_FACE('',(#1193),#8120,.F.);
#8488=ADVANCED_FACE('',(#1194),#766,.T.);
#8489=ADVANCED_FACE('',(#1195),#8121,.F.);
#8490=ADVANCED_FACE('',(#1196),#767,.T.);
#8491=ADVANCED_FACE('',(#1197),#768,.T.);
#8492=ADVANCED_FACE('',(#1198),#769,.T.);
#8493=ADVANCED_FACE('',(#1199),#770,.T.);
#8494=ADVANCED_FACE('',(#1200),#771,.T.);
#8495=ADVANCED_FACE('',(#1201,#455,#456,#457,#458),#772,.T.);
#8496=ADVANCED_FACE('',(#1202),#773,.T.);
#8497=ADVANCED_FACE('',(#1203),#774,.T.);
#8498=ADVANCED_FACE('',(#1204),#775,.T.);
#8499=ADVANCED_FACE('',(#1205),#776,.T.);
#8500=ADVANCED_FACE('',(#1206),#777,.T.);
#8501=ADVANCED_FACE('',(#1207),#778,.T.);
#8502=ADVANCED_FACE('',(#1208),#779,.T.);
#8503=ADVANCED_FACE('',(#1209),#780,.T.);
#8504=ADVANCED_FACE('',(#1210),#781,.T.);
#8505=ADVANCED_FACE('',(#1211),#782,.T.);
#8506=ADVANCED_FACE('',(#1212),#783,.T.);
#8507=ADVANCED_FACE('',(#1213),#784,.T.);
#8508=ADVANCED_FACE('',(#1214),#785,.T.);
#8509=ADVANCED_FACE('',(#1215),#786,.T.);
#8510=ADVANCED_FACE('',(#1216),#787,.T.);
#8511=ADVANCED_FACE('',(#1217),#788,.T.);
#8512=ADVANCED_FACE('',(#1218),#789,.T.);
#8513=ADVANCED_FACE('',(#1219),#790,.F.);
#8514=ADVANCED_FACE('',(#1220),#791,.T.);
#8515=ADVANCED_FACE('',(#1221),#792,.T.);
#8516=ADVANCED_FACE('',(#1222),#793,.T.);
#8517=ADVANCED_FACE('',(#1223),#794,.T.);
#8518=ADVANCED_FACE('',(#1224),#795,.T.);
#8519=ADVANCED_FACE('',(#1225),#796,.T.);
#8520=ADVANCED_FACE('',(#1226),#797,.T.);
#8521=ADVANCED_FACE('',(#1227),#798,.T.);
#8522=ADVANCED_FACE('',(#1228),#799,.T.);
#8523=ADVANCED_FACE('',(#1229),#800,.T.);
#8524=ADVANCED_FACE('',(#1230),#249,.F.);
#8525=ADVANCED_FACE('',(#1231),#8122,.F.);
#8526=ADVANCED_FACE('',(#1232,#459),#801,.T.);
#8527=ADVANCED_FACE('',(#1233),#8123,.T.);
#8528=ADVANCED_FACE('',(#1234,#460),#802,.F.);
#8529=ADVANCED_FACE('',(#1235),#803,.T.);
#8530=ADVANCED_FACE('',(#1236),#250,.T.);
#8531=ADVANCED_FACE('',(#1237),#8124,.T.);
#8532=ADVANCED_FACE('',(#1238),#251,.T.);
#8533=ADVANCED_FACE('',(#1239,#461),#804,.T.);
#8534=ADVANCED_FACE('',(#1240),#252,.T.);
#8535=ADVANCED_FACE('',(#1241),#8125,.T.);
#8536=ADVANCED_FACE('',(#1242),#253,.T.);
#8537=ADVANCED_FACE('',(#1243),#805,.T.);
#8538=ADVANCED_FACE('',(#1244),#806,.F.);
#8539=ADVANCED_FACE('',(#1245),#807,.F.);
#8540=ADVANCED_FACE('',(#1246),#808,.F.);
#8541=ADVANCED_FACE('',(#1247),#809,.F.);
#8542=ADVANCED_FACE('',(#1248),#810,.F.);
#8543=ADVANCED_FACE('',(#1249),#811,.F.);
#8544=ADVANCED_FACE('',(#1250),#812,.F.);
#8545=ADVANCED_FACE('',(#1251),#813,.F.);
#8546=ADVANCED_FACE('',(#1252),#254,.F.);
#8547=ADVANCED_FACE('',(#1253),#8126,.F.);
#8548=ADVANCED_FACE('',(#1254,#462),#814,.T.);
#8549=ADVANCED_FACE('',(#1255),#8127,.T.);
#8550=ADVANCED_FACE('',(#1256,#463),#815,.F.);
#8551=ADVANCED_FACE('',(#1257),#816,.T.);
#8552=ADVANCED_FACE('',(#1258),#255,.T.);
#8553=ADVANCED_FACE('',(#1259),#8128,.T.);
#8554=ADVANCED_FACE('',(#1260),#256,.T.);
#8555=ADVANCED_FACE('',(#1261,#464),#817,.T.);
#8556=ADVANCED_FACE('',(#1262),#257,.T.);
#8557=ADVANCED_FACE('',(#1263),#8129,.T.);
#8558=ADVANCED_FACE('',(#1264),#258,.T.);
#8559=ADVANCED_FACE('',(#1265),#818,.T.);
#8560=ADVANCED_FACE('',(#1266),#819,.F.);
#8561=ADVANCED_FACE('',(#1267),#820,.F.);
#8562=ADVANCED_FACE('',(#1268),#821,.F.);
#8563=ADVANCED_FACE('',(#1269),#822,.F.);
#8564=ADVANCED_FACE('',(#1270),#823,.F.);
#8565=ADVANCED_FACE('',(#1271),#824,.F.);
#8566=ADVANCED_FACE('',(#1272),#825,.F.);
#8567=ADVANCED_FACE('',(#1273),#826,.F.);
#8568=ADVANCED_FACE('',(#1274),#8130,.F.);
#8569=ADVANCED_FACE('',(#1275),#8131,.T.);
#8570=ADVANCED_FACE('',(#1276,#465),#827,.T.);
#8571=ADVANCED_FACE('',(#1277,#466),#828,.F.);
#8572=ADVANCED_FACE('',(#1278),#829,.T.);
#8573=ADVANCED_FACE('',(#1279),#259,.T.);
#8574=ADVANCED_FACE('',(#1280),#8132,.T.);
#8575=ADVANCED_FACE('',(#1281),#260,.T.);
#8576=ADVANCED_FACE('',(#1282,#467),#830,.T.);
#8577=ADVANCED_FACE('',(#1283),#261,.T.);
#8578=ADVANCED_FACE('',(#1284),#8133,.T.);
#8579=ADVANCED_FACE('',(#1285),#262,.T.);
#8580=ADVANCED_FACE('',(#1286),#831,.T.);
#8581=ADVANCED_FACE('',(#1287),#832,.F.);
#8582=ADVANCED_FACE('',(#1288),#833,.F.);
#8583=ADVANCED_FACE('',(#1289),#834,.F.);
#8584=ADVANCED_FACE('',(#1290),#835,.F.);
#8585=ADVANCED_FACE('',(#1291),#836,.F.);
#8586=ADVANCED_FACE('',(#1292),#837,.F.);
#8587=ADVANCED_FACE('',(#1293),#838,.F.);
#8588=ADVANCED_FACE('',(#1294),#839,.F.);
#8589=CLOSED_SHELL('',(#8134,#8135,#8136,#8137,#8138,#8139,#8140,#8141,
#8142,#8143,#8144,#8145,#8146,#8147,#8148,#8149,#8150,#8151,#8152,#8153));
#8590=CLOSED_SHELL('',(#8154,#8155,#8156,#8157,#8158,#8159,#8160,#8161,
#8162,#8163,#8164,#8165));
#8591=CLOSED_SHELL('',(#8166,#8167,#8168,#8169,#8170,#8171));
#8592=CLOSED_SHELL('',(#8172,#8173,#8174,#8175,#8176,#8177,#8178,#8179,
#8180,#8181,#8182,#8183));
#8593=CLOSED_SHELL('',(#8184,#8185,#8186,#8187,#8188,#8189));
#8594=CLOSED_SHELL('',(#8190,#8191,#8192,#8193,#8194,#8195,#8196,#8197,
#8198,#8199,#8200,#8201,#8202,#8203,#8204,#8205,#8206,#8207,#8208,#8209,
#8210,#8211,#8212,#8213,#8214,#8215,#8216,#8217,#8218,#8219,#8220,#8221,
#8222,#8223,#8224,#8225,#8226,#8227,#8228,#8229,#8230,#8231,#8232,#8233,
#8234,#8235,#8236,#8237,#8238,#8239,#8240,#8241,#8242,#8243,#8244,#8245,
#8246,#8247,#8248,#8249,#8250,#8251,#8252,#8253,#8254,#8255,#8256,#8257,
#8258,#8259,#8260,#8261,#8262,#8263,#8264,#8265,#8266,#8267,#8268,#8269,
#8270,#8271,#8272,#8273,#8274,#8275,#8276,#8277,#8278,#8279,#8280,#8281,
#8282,#8283,#8284,#8285,#8286,#8287,#8288,#8289,#8290,#8291,#8292,#8293,
#8294,#8295,#8296,#8297,#8298,#8299,#8300,#8301,#8302,#8303,#8304,#8305,
#8306,#8307,#8308,#8309,#8310,#8311,#8312,#8313));
#8595=CLOSED_SHELL('',(#8314,#8315,#8316,#8317,#8318,#8319));
#8596=CLOSED_SHELL('',(#8320,#8321,#8322,#8323,#8324,#8325));
#8597=CLOSED_SHELL('',(#8326,#8327,#8328,#8329,#8330,#8331));
#8598=CLOSED_SHELL('',(#8332,#8333,#8334,#8335,#8336,#8337));
#8599=CLOSED_SHELL('',(#8338,#8339,#8340,#8341,#8342,#8343,#8344,#8345,
#8346,#8347,#8348,#8349,#8350,#8351,#8352,#8353,#8354,#8355,#8356,#8357,
#8358,#8359,#8360,#8361,#8362,#8363));
#8600=CLOSED_SHELL('',(#8364,#8365,#8366,#8367,#8368,#8369,#8370,#8371,
#8372,#8373,#8374,#8375,#8376,#8377,#8378,#8379,#8380,#8381,#8382,#8383,
#8384,#8385,#8386,#8387,#8388,#8389,#8390,#8391,#8392,#8393,#8394,#8395,
#8396,#8397,#8398,#8399,#8400,#8401,#8402,#8403,#8404,#8405,#8406,#8407,
#8408,#8409,#8410));
#8601=CLOSED_SHELL('',(#8411,#8412,#8413,#8414,#8415,#8416,#8417,#8418,
#8419,#8420,#8421,#8422,#8423,#8424));
#8602=CLOSED_SHELL('',(#8425,#8426,#8427,#8428,#8429,#8430,#8431,#8432));
#8603=CLOSED_SHELL('',(#8433,#8434,#8435,#8436,#8437,#8438,#8439,#8440));
#8604=CLOSED_SHELL('',(#8441,#8442,#8443,#8444,#8445,#8446,#8447,#8448));
#8605=CLOSED_SHELL('',(#8449,#8450,#8451,#8452,#8453,#8454,#8455,#8456));
#8606=CLOSED_SHELL('',(#8457,#8458,#8459,#8460,#8461,#8462,#8463,#8464,
#8465,#8466,#8467,#8468));
#8607=CLOSED_SHELL('',(#8469,#8470,#8471,#8472,#8473,#8474,#8475,#8476,
#8477));
#8608=CLOSED_SHELL('',(#8478,#8479,#8480,#8481));
#8609=CLOSED_SHELL('',(#8482,#8483,#8484,#8485,#8486,#8487,#8488,#8489,
#8490,#8491,#8492,#8493,#8494,#8495,#8496,#8497,#8498,#8499,#8500,#8501,
#8502,#8503));
#8610=CLOSED_SHELL('',(#8504,#8505,#8506,#8507,#8508,#8509,#8510,#8511,
#8512,#8513));
#8611=CLOSED_SHELL('',(#8514,#8515,#8516,#8517,#8518,#8519,#8520,#8521,
#8522,#8523));
#8612=CLOSED_SHELL('',(#8524,#8525,#8526,#8527,#8528));
#8613=CLOSED_SHELL('',(#8529,#8530,#8531,#8532,#8533,#8534,#8535,#8536,
#8537));
#8614=CLOSED_SHELL('',(#8538,#8539,#8540,#8541,#8542,#8543,#8544,#8545));
#8615=CLOSED_SHELL('',(#8546,#8547,#8548,#8549,#8550));
#8616=CLOSED_SHELL('',(#8551,#8552,#8553,#8554,#8555,#8556,#8557,#8558,
#8559));
#8617=CLOSED_SHELL('',(#8560,#8561,#8562,#8563,#8564,#8565,#8566,#8567));
#8618=CLOSED_SHELL('',(#8568,#8569,#8570,#8571));
#8619=CLOSED_SHELL('',(#8572,#8573,#8574,#8575,#8576,#8577,#8578,#8579,
#8580));
#8620=CLOSED_SHELL('',(#8581,#8582,#8583,#8584,#8585,#8586,#8587,#8588));
#8621=DERIVED_UNIT_ELEMENT(#8675,1.);
#8622=DERIVED_UNIT_ELEMENT(#14480,-3.);
#8623=DERIVED_UNIT_ELEMENT(#8675,1.);
#8624=DERIVED_UNIT_ELEMENT(#14480,-3.);
#8625=DERIVED_UNIT_ELEMENT(#8675,1.);
#8626=DERIVED_UNIT_ELEMENT(#14480,-3.);
#8627=DERIVED_UNIT_ELEMENT(#8675,1.);
#8628=DERIVED_UNIT_ELEMENT(#14480,-3.);
#8629=DERIVED_UNIT_ELEMENT(#8675,1.);
#8630=DERIVED_UNIT_ELEMENT(#14480,-3.);
#8631=DERIVED_UNIT_ELEMENT(#8675,1.);
#8632=DERIVED_UNIT_ELEMENT(#14480,-3.);
#8633=DERIVED_UNIT_ELEMENT(#8675,1.);
#8634=DERIVED_UNIT_ELEMENT(#14480,-3.);
#8635=DERIVED_UNIT_ELEMENT(#8675,1.);
#8636=DERIVED_UNIT_ELEMENT(#14480,-3.);
#8637=DERIVED_UNIT_ELEMENT(#8675,1.);
#8638=DERIVED_UNIT_ELEMENT(#14480,-3.);
#8639=DERIVED_UNIT_ELEMENT(#8675,1.);
#8640=DERIVED_UNIT_ELEMENT(#14480,-3.);
#8641=DERIVED_UNIT_ELEMENT(#8675,1.);
#8642=DERIVED_UNIT_ELEMENT(#14480,-3.);
#8643=DERIVED_UNIT_ELEMENT(#8675,1.);
#8644=DERIVED_UNIT_ELEMENT(#14480,-3.);
#8645=DERIVED_UNIT_ELEMENT(#8675,1.);
#8646=DERIVED_UNIT_ELEMENT(#14480,-3.);
#8647=DERIVED_UNIT_ELEMENT(#8675,1.);
#8648=DERIVED_UNIT_ELEMENT(#14480,-3.);
#8649=DERIVED_UNIT_ELEMENT(#8675,1.);
#8650=DERIVED_UNIT_ELEMENT(#14480,-3.);
#8651=DERIVED_UNIT_ELEMENT(#8675,1.);
#8652=DERIVED_UNIT_ELEMENT(#14480,-3.);
#8653=DERIVED_UNIT_ELEMENT(#8675,1.);
#8654=DERIVED_UNIT_ELEMENT(#14480,-3.);
#8655=DERIVED_UNIT_ELEMENT(#8675,1.);
#8656=DERIVED_UNIT_ELEMENT(#14480,-3.);
#8657=DERIVED_UNIT_ELEMENT(#8675,1.);
#8658=DERIVED_UNIT_ELEMENT(#14480,-3.);
#8659=DERIVED_UNIT_ELEMENT(#8675,1.);
#8660=DERIVED_UNIT_ELEMENT(#14480,-3.);
#8661=DERIVED_UNIT_ELEMENT(#8675,1.);
#8662=DERIVED_UNIT_ELEMENT(#14480,-3.);
#8663=DERIVED_UNIT_ELEMENT(#8675,1.);
#8664=DERIVED_UNIT_ELEMENT(#14480,-3.);
#8665=DERIVED_UNIT_ELEMENT(#8675,1.);
#8666=DERIVED_UNIT_ELEMENT(#14480,-3.);
#8667=DERIVED_UNIT_ELEMENT(#8675,1.);
#8668=DERIVED_UNIT_ELEMENT(#14480,-3.);
#8669=DERIVED_UNIT_ELEMENT(#8675,1.);
#8670=DERIVED_UNIT_ELEMENT(#14480,-3.);
#8671=DERIVED_UNIT_ELEMENT(#8675,1.);
#8672=DERIVED_UNIT_ELEMENT(#14480,-3.);
#8673=DERIVED_UNIT_ELEMENT(#8675,1.);
#8674=DERIVED_UNIT_ELEMENT(#14480,-3.);
#8675=(
MASS_UNIT()
NAMED_UNIT(*)
SI_UNIT(.KILO.,.GRAM.)
);
#8676=DERIVED_UNIT((#8621,#8622));
#8677=DERIVED_UNIT((#8623,#8624));
#8678=DERIVED_UNIT((#8625,#8626));
#8679=DERIVED_UNIT((#8627,#8628));
#8680=DERIVED_UNIT((#8629,#8630));
#8681=DERIVED_UNIT((#8631,#8632));
#8682=DERIVED_UNIT((#8633,#8634));
#8683=DERIVED_UNIT((#8635,#8636));
#8684=DERIVED_UNIT((#8637,#8638));
#8685=DERIVED_UNIT((#8639,#8640));
#8686=DERIVED_UNIT((#8641,#8642));
#8687=DERIVED_UNIT((#8643,#8644));
#8688=DERIVED_UNIT((#8645,#8646));
#8689=DERIVED_UNIT((#8647,#8648));
#8690=DERIVED_UNIT((#8649,#8650));
#8691=DERIVED_UNIT((#8651,#8652));
#8692=DERIVED_UNIT((#8653,#8654));
#8693=DERIVED_UNIT((#8655,#8656));
#8694=DERIVED_UNIT((#8657,#8658));
#8695=DERIVED_UNIT((#8659,#8660));
#8696=DERIVED_UNIT((#8661,#8662));
#8697=DERIVED_UNIT((#8663,#8664));
#8698=DERIVED_UNIT((#8665,#8666));
#8699=DERIVED_UNIT((#8667,#8668));
#8700=DERIVED_UNIT((#8669,#8670));
#8701=DERIVED_UNIT((#8671,#8672));
#8702=DERIVED_UNIT((#8673,#8674));
#8703=MEASURE_REPRESENTATION_ITEM('density measure',
POSITIVE_RATIO_MEASURE(7850.),#8676);
#8704=MEASURE_REPRESENTATION_ITEM('density measure',
POSITIVE_RATIO_MEASURE(7850.),#8677);
#8705=MEASURE_REPRESENTATION_ITEM('density measure',
POSITIVE_RATIO_MEASURE(7850.),#8678);
#8706=MEASURE_REPRESENTATION_ITEM('density measure',
POSITIVE_RATIO_MEASURE(7850.),#8679);
#8707=MEASURE_REPRESENTATION_ITEM('density measure',
POSITIVE_RATIO_MEASURE(7850.),#8680);
#8708=MEASURE_REPRESENTATION_ITEM('density measure',
POSITIVE_RATIO_MEASURE(7850.),#8681);
#8709=MEASURE_REPRESENTATION_ITEM('density measure',
POSITIVE_RATIO_MEASURE(7850.),#8682);
#8710=MEASURE_REPRESENTATION_ITEM('density measure',
POSITIVE_RATIO_MEASURE(7850.),#8683);
#8711=MEASURE_REPRESENTATION_ITEM('density measure',
POSITIVE_RATIO_MEASURE(7850.),#8684);
#8712=MEASURE_REPRESENTATION_ITEM('density measure',
POSITIVE_RATIO_MEASURE(7850.),#8685);
#8713=MEASURE_REPRESENTATION_ITEM('density measure',
POSITIVE_RATIO_MEASURE(7850.),#8686);
#8714=MEASURE_REPRESENTATION_ITEM('density measure',
POSITIVE_RATIO_MEASURE(7850.),#8687);
#8715=MEASURE_REPRESENTATION_ITEM('density measure',
POSITIVE_RATIO_MEASURE(7850.),#8688);
#8716=MEASURE_REPRESENTATION_ITEM('density measure',
POSITIVE_RATIO_MEASURE(7850.),#8689);
#8717=MEASURE_REPRESENTATION_ITEM('density measure',
POSITIVE_RATIO_MEASURE(7850.),#8690);
#8718=MEASURE_REPRESENTATION_ITEM('density measure',
POSITIVE_RATIO_MEASURE(7850.),#8691);
#8719=MEASURE_REPRESENTATION_ITEM('density measure',
POSITIVE_RATIO_MEASURE(7850.),#8692);
#8720=MEASURE_REPRESENTATION_ITEM('density measure',
POSITIVE_RATIO_MEASURE(7850.),#8693);
#8721=MEASURE_REPRESENTATION_ITEM('density measure',
POSITIVE_RATIO_MEASURE(7850.),#8694);
#8722=MEASURE_REPRESENTATION_ITEM('density measure',
POSITIVE_RATIO_MEASURE(7850.),#8695);
#8723=MEASURE_REPRESENTATION_ITEM('density measure',
POSITIVE_RATIO_MEASURE(7850.),#8696);
#8724=MEASURE_REPRESENTATION_ITEM('density measure',
POSITIVE_RATIO_MEASURE(7850.),#8697);
#8725=MEASURE_REPRESENTATION_ITEM('density measure',
POSITIVE_RATIO_MEASURE(7850.),#8698);
#8726=MEASURE_REPRESENTATION_ITEM('density measure',
POSITIVE_RATIO_MEASURE(7850.),#8699);
#8727=MEASURE_REPRESENTATION_ITEM('density measure',
POSITIVE_RATIO_MEASURE(7850.),#8700);
#8728=MEASURE_REPRESENTATION_ITEM('density measure',
POSITIVE_RATIO_MEASURE(7850.),#8701);
#8729=MEASURE_REPRESENTATION_ITEM('density measure',
POSITIVE_RATIO_MEASURE(7850.),#8702);
#8730=PROPERTY_DEFINITION_REPRESENTATION(#8865,#8784);
#8731=PROPERTY_DEFINITION_REPRESENTATION(#8866,#8785);
#8732=PROPERTY_DEFINITION_REPRESENTATION(#8867,#8786);
#8733=PROPERTY_DEFINITION_REPRESENTATION(#8868,#8787);
#8734=PROPERTY_DEFINITION_REPRESENTATION(#8869,#8788);
#8735=PROPERTY_DEFINITION_REPRESENTATION(#8870,#8789);
#8736=PROPERTY_DEFINITION_REPRESENTATION(#8871,#8790);
#8737=PROPERTY_DEFINITION_REPRESENTATION(#8872,#8791);
#8738=PROPERTY_DEFINITION_REPRESENTATION(#8873,#8792);
#8739=PROPERTY_DEFINITION_REPRESENTATION(#8874,#8793);
#8740=PROPERTY_DEFINITION_REPRESENTATION(#8875,#8794);
#8741=PROPERTY_DEFINITION_REPRESENTATION(#8876,#8795);
#8742=PROPERTY_DEFINITION_REPRESENTATION(#8877,#8796);
#8743=PROPERTY_DEFINITION_REPRESENTATION(#8878,#8797);
#8744=PROPERTY_DEFINITION_REPRESENTATION(#8879,#8798);
#8745=PROPERTY_DEFINITION_REPRESENTATION(#8880,#8799);
#8746=PROPERTY_DEFINITION_REPRESENTATION(#8881,#8800);
#8747=PROPERTY_DEFINITION_REPRESENTATION(#8882,#8801);
#8748=PROPERTY_DEFINITION_REPRESENTATION(#8883,#8802);
#8749=PROPERTY_DEFINITION_REPRESENTATION(#8884,#8803);
#8750=PROPERTY_DEFINITION_REPRESENTATION(#8885,#8804);
#8751=PROPERTY_DEFINITION_REPRESENTATION(#8886,#8805);
#8752=PROPERTY_DEFINITION_REPRESENTATION(#8887,#8806);
#8753=PROPERTY_DEFINITION_REPRESENTATION(#8888,#8807);
#8754=PROPERTY_DEFINITION_REPRESENTATION(#8889,#8808);
#8755=PROPERTY_DEFINITION_REPRESENTATION(#8890,#8809);
#8756=PROPERTY_DEFINITION_REPRESENTATION(#8891,#8810);
#8757=PROPERTY_DEFINITION_REPRESENTATION(#8892,#8811);
#8758=PROPERTY_DEFINITION_REPRESENTATION(#8893,#8812);
#8759=PROPERTY_DEFINITION_REPRESENTATION(#8894,#8813);
#8760=PROPERTY_DEFINITION_REPRESENTATION(#8895,#8814);
#8761=PROPERTY_DEFINITION_REPRESENTATION(#8896,#8815);
#8762=PROPERTY_DEFINITION_REPRESENTATION(#8897,#8816);
#8763=PROPERTY_DEFINITION_REPRESENTATION(#8898,#8817);
#8764=PROPERTY_DEFINITION_REPRESENTATION(#8899,#8818);
#8765=PROPERTY_DEFINITION_REPRESENTATION(#8900,#8819);
#8766=PROPERTY_DEFINITION_REPRESENTATION(#8901,#8820);
#8767=PROPERTY_DEFINITION_REPRESENTATION(#8902,#8821);
#8768=PROPERTY_DEFINITION_REPRESENTATION(#8903,#8822);
#8769=PROPERTY_DEFINITION_REPRESENTATION(#8904,#8823);
#8770=PROPERTY_DEFINITION_REPRESENTATION(#8905,#8824);
#8771=PROPERTY_DEFINITION_REPRESENTATION(#8906,#8825);
#8772=PROPERTY_DEFINITION_REPRESENTATION(#8907,#8826);
#8773=PROPERTY_DEFINITION_REPRESENTATION(#8908,#8827);
#8774=PROPERTY_DEFINITION_REPRESENTATION(#8909,#8828);
#8775=PROPERTY_DEFINITION_REPRESENTATION(#8910,#8829);
#8776=PROPERTY_DEFINITION_REPRESENTATION(#8911,#8830);
#8777=PROPERTY_DEFINITION_REPRESENTATION(#8912,#8831);
#8778=PROPERTY_DEFINITION_REPRESENTATION(#8913,#8832);
#8779=PROPERTY_DEFINITION_REPRESENTATION(#8914,#8833);
#8780=PROPERTY_DEFINITION_REPRESENTATION(#8915,#8834);
#8781=PROPERTY_DEFINITION_REPRESENTATION(#8916,#8835);
#8782=PROPERTY_DEFINITION_REPRESENTATION(#8917,#8836);
#8783=PROPERTY_DEFINITION_REPRESENTATION(#8918,#8837);
#8784=REPRESENTATION('material name',(#8838),#14449);
#8785=REPRESENTATION('density',(#8703),#14449);
#8786=REPRESENTATION('material name',(#8839),#14450);
#8787=REPRESENTATION('density',(#8704),#14450);
#8788=REPRESENTATION('material name',(#8840),#14451);
#8789=REPRESENTATION('density',(#8705),#14451);
#8790=REPRESENTATION('material name',(#8841),#14452);
#8791=REPRESENTATION('density',(#8706),#14452);
#8792=REPRESENTATION('material name',(#8842),#14453);
#8793=REPRESENTATION('density',(#8707),#14453);
#8794=REPRESENTATION('material name',(#8843),#14454);
#8795=REPRESENTATION('density',(#8708),#14454);
#8796=REPRESENTATION('material name',(#8844),#14455);
#8797=REPRESENTATION('density',(#8709),#14455);
#8798=REPRESENTATION('material name',(#8845),#14456);
#8799=REPRESENTATION('density',(#8710),#14456);
#8800=REPRESENTATION('material name',(#8846),#14457);
#8801=REPRESENTATION('density',(#8711),#14457);
#8802=REPRESENTATION('material name',(#8847),#14458);
#8803=REPRESENTATION('density',(#8712),#14458);
#8804=REPRESENTATION('material name',(#8848),#14459);
#8805=REPRESENTATION('density',(#8713),#14459);
#8806=REPRESENTATION('material name',(#8849),#14460);
#8807=REPRESENTATION('density',(#8714),#14460);
#8808=REPRESENTATION('material name',(#8850),#14461);
#8809=REPRESENTATION('density',(#8715),#14461);
#8810=REPRESENTATION('material name',(#8851),#14462);
#8811=REPRESENTATION('density',(#8716),#14462);
#8812=REPRESENTATION('material name',(#8852),#14463);
#8813=REPRESENTATION('density',(#8717),#14463);
#8814=REPRESENTATION('material name',(#8853),#14465);
#8815=REPRESENTATION('density',(#8718),#14465);
#8816=REPRESENTATION('material name',(#8854),#14466);
#8817=REPRESENTATION('density',(#8719),#14466);
#8818=REPRESENTATION('material name',(#8855),#14467);
#8819=REPRESENTATION('density',(#8720),#14467);
#8820=REPRESENTATION('material name',(#8856),#14469);
#8821=REPRESENTATION('density',(#8721),#14469);
#8822=REPRESENTATION('material name',(#8857),#14470);
#8823=REPRESENTATION('density',(#8722),#14470);
#8824=REPRESENTATION('material name',(#8858),#14471);
#8825=REPRESENTATION('density',(#8723),#14471);
#8826=REPRESENTATION('material name',(#8859),#14472);
#8827=REPRESENTATION('density',(#8724),#14472);
#8828=REPRESENTATION('material name',(#8860),#14473);
#8829=REPRESENTATION('density',(#8725),#14473);
#8830=REPRESENTATION('material name',(#8861),#14474);
#8831=REPRESENTATION('density',(#8726),#14474);
#8832=REPRESENTATION('material name',(#8862),#14475);
#8833=REPRESENTATION('density',(#8727),#14475);
#8834=REPRESENTATION('material name',(#8863),#14476);
#8835=REPRESENTATION('density',(#8728),#14476);
#8836=REPRESENTATION('material name',(#8864),#14477);
#8837=REPRESENTATION('density',(#8729),#14477);
#8838=DESCRIPTIVE_REPRESENTATION_ITEM('Steel','Steel');
#8839=DESCRIPTIVE_REPRESENTATION_ITEM('Steel','Steel');
#8840=DESCRIPTIVE_REPRESENTATION_ITEM('Steel','Steel');
#8841=DESCRIPTIVE_REPRESENTATION_ITEM('Steel','Steel');
#8842=DESCRIPTIVE_REPRESENTATION_ITEM('Steel','Steel');
#8843=DESCRIPTIVE_REPRESENTATION_ITEM('Steel','Steel');
#8844=DESCRIPTIVE_REPRESENTATION_ITEM('Steel','Steel');
#8845=DESCRIPTIVE_REPRESENTATION_ITEM('Steel','Steel');
#8846=DESCRIPTIVE_REPRESENTATION_ITEM('Steel','Steel');
#8847=DESCRIPTIVE_REPRESENTATION_ITEM('Steel','Steel');
#8848=DESCRIPTIVE_REPRESENTATION_ITEM('Steel','Steel');
#8849=DESCRIPTIVE_REPRESENTATION_ITEM('Steel','Steel');
#8850=DESCRIPTIVE_REPRESENTATION_ITEM('Steel','Steel');
#8851=DESCRIPTIVE_REPRESENTATION_ITEM('Steel','Steel');
#8852=DESCRIPTIVE_REPRESENTATION_ITEM('Steel','Steel');
#8853=DESCRIPTIVE_REPRESENTATION_ITEM('Steel','Steel');
#8854=DESCRIPTIVE_REPRESENTATION_ITEM('Steel','Steel');
#8855=DESCRIPTIVE_REPRESENTATION_ITEM('Steel','Steel');
#8856=DESCRIPTIVE_REPRESENTATION_ITEM('Steel','Steel');
#8857=DESCRIPTIVE_REPRESENTATION_ITEM('Steel','Steel');
#8858=DESCRIPTIVE_REPRESENTATION_ITEM('Steel','Steel');
#8859=DESCRIPTIVE_REPRESENTATION_ITEM('Steel','Steel');
#8860=DESCRIPTIVE_REPRESENTATION_ITEM('Steel','Steel');
#8861=DESCRIPTIVE_REPRESENTATION_ITEM('Steel','Steel');
#8862=DESCRIPTIVE_REPRESENTATION_ITEM('Steel','Steel');
#8863=DESCRIPTIVE_REPRESENTATION_ITEM('Steel','Steel');
#8864=DESCRIPTIVE_REPRESENTATION_ITEM('Steel','Steel');
#8865=PROPERTY_DEFINITION('material property','material name',#14637);
#8866=PROPERTY_DEFINITION('material property','density of part',#14637);
#8867=PROPERTY_DEFINITION('material property','material name',#14638);
#8868=PROPERTY_DEFINITION('material property','density of part',#14638);
#8869=PROPERTY_DEFINITION('material property','material name',#14639);
#8870=PROPERTY_DEFINITION('material property','density of part',#14639);
#8871=PROPERTY_DEFINITION('material property','material name',#14640);
#8872=PROPERTY_DEFINITION('material property','density of part',#14640);
#8873=PROPERTY_DEFINITION('material property','material name',#14641);
#8874=PROPERTY_DEFINITION('material property','density of part',#14641);
#8875=PROPERTY_DEFINITION('material property','material name',#14642);
#8876=PROPERTY_DEFINITION('material property','density of part',#14642);
#8877=PROPERTY_DEFINITION('material property','material name',#14643);
#8878=PROPERTY_DEFINITION('material property','density of part',#14643);
#8879=PROPERTY_DEFINITION('material property','material name',#14644);
#8880=PROPERTY_DEFINITION('material property','density of part',#14644);
#8881=PROPERTY_DEFINITION('material property','material name',#14645);
#8882=PROPERTY_DEFINITION('material property','density of part',#14645);
#8883=PROPERTY_DEFINITION('material property','material name',#14646);
#8884=PROPERTY_DEFINITION('material property','density of part',#14646);
#8885=PROPERTY_DEFINITION('material property','material name',#14647);
#8886=PROPERTY_DEFINITION('material property','density of part',#14647);
#8887=PROPERTY_DEFINITION('material property','material name',#14648);
#8888=PROPERTY_DEFINITION('material property','density of part',#14648);
#8889=PROPERTY_DEFINITION('material property','material name',#14649);
#8890=PROPERTY_DEFINITION('material property','density of part',#14649);
#8891=PROPERTY_DEFINITION('material property','material name',#14650);
#8892=PROPERTY_DEFINITION('material property','density of part',#14650);
#8893=PROPERTY_DEFINITION('material property','material name',#14651);
#8894=PROPERTY_DEFINITION('material property','density of part',#14651);
#8895=PROPERTY_DEFINITION('material property','material name',#14653);
#8896=PROPERTY_DEFINITION('material property','density of part',#14653);
#8897=PROPERTY_DEFINITION('material property','material name',#14654);
#8898=PROPERTY_DEFINITION('material property','density of part',#14654);
#8899=PROPERTY_DEFINITION('material property','material name',#14655);
#8900=PROPERTY_DEFINITION('material property','density of part',#14655);
#8901=PROPERTY_DEFINITION('material property','material name',#14657);
#8902=PROPERTY_DEFINITION('material property','density of part',#14657);
#8903=PROPERTY_DEFINITION('material property','material name',#14658);
#8904=PROPERTY_DEFINITION('material property','density of part',#14658);
#8905=PROPERTY_DEFINITION('material property','material name',#14659);
#8906=PROPERTY_DEFINITION('material property','density of part',#14659);
#8907=PROPERTY_DEFINITION('material property','material name',#14660);
#8908=PROPERTY_DEFINITION('material property','density of part',#14660);
#8909=PROPERTY_DEFINITION('material property','material name',#14661);
#8910=PROPERTY_DEFINITION('material property','density of part',#14661);
#8911=PROPERTY_DEFINITION('material property','material name',#14662);
#8912=PROPERTY_DEFINITION('material property','density of part',#14662);
#8913=PROPERTY_DEFINITION('material property','material name',#14663);
#8914=PROPERTY_DEFINITION('material property','density of part',#14663);
#8915=PROPERTY_DEFINITION('material property','material name',#14664);
#8916=PROPERTY_DEFINITION('material property','density of part',#14664);
#8917=PROPERTY_DEFINITION('material property','material name',#14665);
#8918=PROPERTY_DEFINITION('material property','density of part',#14665);
#8919=AXIS2_PLACEMENT_3D('',#11996,#9621,#9622);
#8920=AXIS2_PLACEMENT_3D('',#11997,#9623,#9624);
#8921=AXIS2_PLACEMENT_3D('',#11998,#9625,#9626);
#8922=AXIS2_PLACEMENT_3D('',#11999,#9627,#9628);
#8923=AXIS2_PLACEMENT_3D('',#12001,#9629,#9630);
#8924=AXIS2_PLACEMENT_3D('',#12004,#9632,#9633);
#8925=AXIS2_PLACEMENT_3D('',#12005,#9634,#9635);
#8926=AXIS2_PLACEMENT_3D('',#12007,#9636,#9637);
#8927=AXIS2_PLACEMENT_3D('',#12010,#9639,#9640);
#8928=AXIS2_PLACEMENT_3D('',#12011,#9641,#9642);
#8929=AXIS2_PLACEMENT_3D('',#12013,#9643,#9644);
#8930=AXIS2_PLACEMENT_3D('',#12016,#9646,#9647);
#8931=AXIS2_PLACEMENT_3D('',#12017,#9648,#9649);
#8932=AXIS2_PLACEMENT_3D('',#12019,#9650,#9651);
#8933=AXIS2_PLACEMENT_3D('',#12022,#9653,#9654);
#8934=AXIS2_PLACEMENT_3D('',#12023,#9655,#9656);
#8935=AXIS2_PLACEMENT_3D('',#12025,#9657,#9658);
#8936=AXIS2_PLACEMENT_3D('',#12028,#9660,#9661);
#8937=AXIS2_PLACEMENT_3D('',#12029,#9662,#9663);
#8938=AXIS2_PLACEMENT_3D('',#12031,#9664,#9665);
#8939=AXIS2_PLACEMENT_3D('',#12034,#9667,#9668);
#8940=AXIS2_PLACEMENT_3D('',#12035,#9669,#9670);
#8941=AXIS2_PLACEMENT_3D('',#12037,#9671,#9672);
#8942=AXIS2_PLACEMENT_3D('',#12040,#9674,#9675);
#8943=AXIS2_PLACEMENT_3D('',#12041,#9676,#9677);
#8944=AXIS2_PLACEMENT_3D('',#12043,#9678,#9679);
#8945=AXIS2_PLACEMENT_3D('',#12046,#9681,#9682);
#8946=AXIS2_PLACEMENT_3D('',#12047,#9683,#9684);
#8947=AXIS2_PLACEMENT_3D('',#12049,#9685,#9686);
#8948=AXIS2_PLACEMENT_3D('',#12052,#9688,#9689);
#8949=AXIS2_PLACEMENT_3D('',#12053,#9690,#9691);
#8950=AXIS2_PLACEMENT_3D('',#12055,#9692,#9693);
#8951=AXIS2_PLACEMENT_3D('',#12058,#9695,#9696);
#8952=AXIS2_PLACEMENT_3D('',#12059,#9697,#9698);
#8953=AXIS2_PLACEMENT_3D('',#12061,#9699,#9700);
#8954=AXIS2_PLACEMENT_3D('',#12064,#9702,#9703);
#8955=AXIS2_PLACEMENT_3D('',#12065,#9704,#9705);
#8956=AXIS2_PLACEMENT_3D('',#12067,#9706,#9707);
#8957=AXIS2_PLACEMENT_3D('',#12070,#9709,#9710);
#8958=AXIS2_PLACEMENT_3D('',#12071,#9711,#9712);
#8959=AXIS2_PLACEMENT_3D('',#12073,#9713,#9714);
#8960=AXIS2_PLACEMENT_3D('',#12076,#9716,#9717);
#8961=AXIS2_PLACEMENT_3D('',#12077,#9718,#9719);
#8962=AXIS2_PLACEMENT_3D('',#12079,#9720,#9721);
#8963=AXIS2_PLACEMENT_3D('',#12082,#9723,#9724);
#8964=AXIS2_PLACEMENT_3D('',#12083,#9725,#9726);
#8965=AXIS2_PLACEMENT_3D('',#12092,#9731,#9732);
#8966=AXIS2_PLACEMENT_3D('',#12098,#9736,#9737);
#8967=AXIS2_PLACEMENT_3D('',#12104,#9741,#9742);
#8968=AXIS2_PLACEMENT_3D('',#12107,#9745,#9746);
#8969=AXIS2_PLACEMENT_3D('',#12108,#9747,#9748);
#8970=AXIS2_PLACEMENT_3D('',#12109,#9749,#9750);
#8971=AXIS2_PLACEMENT_3D('',#12110,#9751,#9752);
#8972=AXIS2_PLACEMENT_3D('',#12112,#9753,#9754);
#8973=AXIS2_PLACEMENT_3D('',#12115,#9756,#9757);
#8974=AXIS2_PLACEMENT_3D('',#12116,#9758,#9759);
#8975=AXIS2_PLACEMENT_3D('',#12118,#9760,#9761);
#8976=AXIS2_PLACEMENT_3D('',#12119,#9762,#9763);
#8977=AXIS2_PLACEMENT_3D('',#12121,#9764,#9765);
#8978=AXIS2_PLACEMENT_3D('',#12124,#9767,#9768);
#8979=AXIS2_PLACEMENT_3D('',#12125,#9769,#9770);
#8980=AXIS2_PLACEMENT_3D('',#12127,#9771,#9772);
#8981=AXIS2_PLACEMENT_3D('',#12128,#9773,#9774);
#8982=AXIS2_PLACEMENT_3D('',#12130,#9775,#9776);
#8983=AXIS2_PLACEMENT_3D('',#12132,#9778,#9779);
#8984=AXIS2_PLACEMENT_3D('',#12134,#9780,#9781);
#8985=AXIS2_PLACEMENT_3D('',#12136,#9783,#9784);
#8986=AXIS2_PLACEMENT_3D('',#12145,#9789,#9790);
#8987=AXIS2_PLACEMENT_3D('',#12151,#9794,#9795);
#8988=AXIS2_PLACEMENT_3D('',#12157,#9799,#9800);
#8989=AXIS2_PLACEMENT_3D('',#12160,#9803,#9804);
#8990=AXIS2_PLACEMENT_3D('',#12161,#9805,#9806);
#8991=AXIS2_PLACEMENT_3D('',#12162,#9807,#9808);
#8992=AXIS2_PLACEMENT_3D('',#12163,#9809,#9810);
#8993=AXIS2_PLACEMENT_3D('',#12172,#9815,#9816);
#8994=AXIS2_PLACEMENT_3D('',#12178,#9820,#9821);
#8995=AXIS2_PLACEMENT_3D('',#12184,#9825,#9826);
#8996=AXIS2_PLACEMENT_3D('',#12187,#9829,#9830);
#8997=AXIS2_PLACEMENT_3D('',#12188,#9831,#9832);
#8998=AXIS2_PLACEMENT_3D('',#12189,#9833,#9834);
#8999=AXIS2_PLACEMENT_3D('',#12190,#9835,#9836);
#9000=AXIS2_PLACEMENT_3D('',#12192,#9837,#9838);
#9001=AXIS2_PLACEMENT_3D('',#12195,#9840,#9841);
#9002=AXIS2_PLACEMENT_3D('',#12196,#9842,#9843);
#9003=AXIS2_PLACEMENT_3D('',#12198,#9844,#9845);
#9004=AXIS2_PLACEMENT_3D('',#12199,#9846,#9847);
#9005=AXIS2_PLACEMENT_3D('',#12201,#9848,#9849);
#9006=AXIS2_PLACEMENT_3D('',#12204,#9851,#9852);
#9007=AXIS2_PLACEMENT_3D('',#12205,#9853,#9854);
#9008=AXIS2_PLACEMENT_3D('',#12207,#9855,#9856);
#9009=AXIS2_PLACEMENT_3D('',#12208,#9857,#9858);
#9010=AXIS2_PLACEMENT_3D('',#12210,#9859,#9860);
#9011=AXIS2_PLACEMENT_3D('',#12212,#9862,#9863);
#9012=AXIS2_PLACEMENT_3D('',#12214,#9864,#9865);
#9013=AXIS2_PLACEMENT_3D('',#12216,#9867,#9868);
#9014=AXIS2_PLACEMENT_3D('',#12225,#9873,#9874);
#9015=AXIS2_PLACEMENT_3D('',#12231,#9878,#9879);
#9016=AXIS2_PLACEMENT_3D('',#12237,#9883,#9884);
#9017=AXIS2_PLACEMENT_3D('',#12240,#9887,#9888);
#9018=AXIS2_PLACEMENT_3D('',#12241,#9889,#9890);
#9019=AXIS2_PLACEMENT_3D('',#12242,#9891,#9892);
#9020=AXIS2_PLACEMENT_3D('',#12243,#9893,#9894);
#9021=AXIS2_PLACEMENT_3D('',#12252,#9899,#9900);
#9022=AXIS2_PLACEMENT_3D('',#12258,#9904,#9905);
#9023=AXIS2_PLACEMENT_3D('',#12264,#9909,#9910);
#9024=AXIS2_PLACEMENT_3D('',#12267,#9913,#9914);
#9025=AXIS2_PLACEMENT_3D('',#12268,#9915,#9916);
#9026=AXIS2_PLACEMENT_3D('',#12269,#9917,#9918);
#9027=AXIS2_PLACEMENT_3D('',#12270,#9919,#9920);
#9028=AXIS2_PLACEMENT_3D('',#12279,#9925,#9926);
#9029=AXIS2_PLACEMENT_3D('',#12285,#9930,#9931);
#9030=AXIS2_PLACEMENT_3D('',#12291,#9935,#9936);
#9031=AXIS2_PLACEMENT_3D('',#12293,#9938,#9939);
#9032=AXIS2_PLACEMENT_3D('',#12302,#9944,#9945);
#9033=AXIS2_PLACEMENT_3D('',#12308,#9949,#9950);
#9034=AXIS2_PLACEMENT_3D('',#12314,#9954,#9955);
#9035=AXIS2_PLACEMENT_3D('',#12316,#9957,#9958);
#9036=AXIS2_PLACEMENT_3D('',#12325,#9963,#9964);
#9037=AXIS2_PLACEMENT_3D('',#12331,#9968,#9969);
#9038=AXIS2_PLACEMENT_3D('',#12337,#9973,#9974);
#9039=AXIS2_PLACEMENT_3D('',#12339,#9976,#9977);
#9040=AXIS2_PLACEMENT_3D('',#12348,#9982,#9983);
#9041=AXIS2_PLACEMENT_3D('',#12354,#9987,#9988);
#9042=AXIS2_PLACEMENT_3D('',#12360,#9992,#9993);
#9043=AXIS2_PLACEMENT_3D('',#12362,#9995,#9996);
#9044=AXIS2_PLACEMENT_3D('',#12371,#10001,#10002);
#9045=AXIS2_PLACEMENT_3D('',#12377,#10006,#10007);
#9046=AXIS2_PLACEMENT_3D('',#12383,#10011,#10012);
#9047=AXIS2_PLACEMENT_3D('',#12385,#10014,#10015);
#9048=AXIS2_PLACEMENT_3D('',#12394,#10020,#10021);
#9049=AXIS2_PLACEMENT_3D('',#12400,#10025,#10026);
#9050=AXIS2_PLACEMENT_3D('',#12406,#10030,#10031);
#9051=AXIS2_PLACEMENT_3D('',#12408,#10033,#10034);
#9052=AXIS2_PLACEMENT_3D('',#12417,#10039,#10040);
#9053=AXIS2_PLACEMENT_3D('',#12423,#10044,#10045);
#9054=AXIS2_PLACEMENT_3D('',#12429,#10049,#10050);
#9055=AXIS2_PLACEMENT_3D('',#12431,#10052,#10053);
#9056=AXIS2_PLACEMENT_3D('',#12440,#10058,#10059);
#9057=AXIS2_PLACEMENT_3D('',#12446,#10063,#10064);
#9058=AXIS2_PLACEMENT_3D('',#12452,#10068,#10069);
#9059=AXIS2_PLACEMENT_3D('',#12454,#10071,#10072);
#9060=AXIS2_PLACEMENT_3D('',#12463,#10077,#10078);
#9061=AXIS2_PLACEMENT_3D('',#12469,#10082,#10083);
#9062=AXIS2_PLACEMENT_3D('',#12475,#10087,#10088);
#9063=AXIS2_PLACEMENT_3D('',#12477,#10090,#10091);
#9064=AXIS2_PLACEMENT_3D('',#12486,#10096,#10097);
#9065=AXIS2_PLACEMENT_3D('',#12492,#10101,#10102);
#9066=AXIS2_PLACEMENT_3D('',#12498,#10106,#10107);
#9067=AXIS2_PLACEMENT_3D('',#12500,#10109,#10110);
#9068=AXIS2_PLACEMENT_3D('',#12509,#10115,#10116);
#9069=AXIS2_PLACEMENT_3D('',#12515,#10120,#10121);
#9070=AXIS2_PLACEMENT_3D('',#12521,#10125,#10126);
#9071=AXIS2_PLACEMENT_3D('',#12523,#10128,#10129);
#9072=AXIS2_PLACEMENT_3D('',#12532,#10134,#10135);
#9073=AXIS2_PLACEMENT_3D('',#12538,#10139,#10140);
#9074=AXIS2_PLACEMENT_3D('',#12544,#10144,#10145);
#9075=AXIS2_PLACEMENT_3D('',#12546,#10147,#10148);
#9076=AXIS2_PLACEMENT_3D('',#12555,#10153,#10154);
#9077=AXIS2_PLACEMENT_3D('',#12561,#10158,#10159);
#9078=AXIS2_PLACEMENT_3D('',#12567,#10163,#10164);
#9079=AXIS2_PLACEMENT_3D('',#12569,#10166,#10167);
#9080=AXIS2_PLACEMENT_3D('',#12578,#10172,#10173);
#9081=AXIS2_PLACEMENT_3D('',#12584,#10177,#10178);
#9082=AXIS2_PLACEMENT_3D('',#12590,#10182,#10183);
#9083=AXIS2_PLACEMENT_3D('',#12592,#10185,#10186);
#9084=AXIS2_PLACEMENT_3D('',#12601,#10191,#10192);
#9085=AXIS2_PLACEMENT_3D('',#12607,#10196,#10197);
#9086=AXIS2_PLACEMENT_3D('',#12613,#10201,#10202);
#9087=AXIS2_PLACEMENT_3D('',#12615,#10204,#10205);
#9088=AXIS2_PLACEMENT_3D('',#12624,#10210,#10211);
#9089=AXIS2_PLACEMENT_3D('',#12630,#10215,#10216);
#9090=AXIS2_PLACEMENT_3D('',#12636,#10220,#10221);
#9091=AXIS2_PLACEMENT_3D('',#12638,#10223,#10224);
#9092=AXIS2_PLACEMENT_3D('',#12647,#10229,#10230);
#9093=AXIS2_PLACEMENT_3D('',#12653,#10234,#10235);
#9094=AXIS2_PLACEMENT_3D('',#12659,#10239,#10240);
#9095=AXIS2_PLACEMENT_3D('',#12661,#10242,#10243);
#9096=AXIS2_PLACEMENT_3D('',#12670,#10248,#10249);
#9097=AXIS2_PLACEMENT_3D('',#12676,#10253,#10254);
#9098=AXIS2_PLACEMENT_3D('',#12682,#10258,#10259);
#9099=AXIS2_PLACEMENT_3D('',#12684,#10261,#10262);
#9100=AXIS2_PLACEMENT_3D('',#12693,#10267,#10268);
#9101=AXIS2_PLACEMENT_3D('',#12699,#10272,#10273);
#9102=AXIS2_PLACEMENT_3D('',#12705,#10277,#10278);
#9103=AXIS2_PLACEMENT_3D('',#12707,#10280,#10281);
#9104=AXIS2_PLACEMENT_3D('',#12716,#10286,#10287);
#9105=AXIS2_PLACEMENT_3D('',#12722,#10291,#10292);
#9106=AXIS2_PLACEMENT_3D('',#12728,#10296,#10297);
#9107=AXIS2_PLACEMENT_3D('',#12730,#10299,#10300);
#9108=AXIS2_PLACEMENT_3D('',#12739,#10305,#10306);
#9109=AXIS2_PLACEMENT_3D('',#12745,#10310,#10311);
#9110=AXIS2_PLACEMENT_3D('',#12751,#10315,#10316);
#9111=AXIS2_PLACEMENT_3D('',#12753,#10318,#10319);
#9112=AXIS2_PLACEMENT_3D('',#12762,#10324,#10325);
#9113=AXIS2_PLACEMENT_3D('',#12768,#10329,#10330);
#9114=AXIS2_PLACEMENT_3D('',#12774,#10334,#10335);
#9115=AXIS2_PLACEMENT_3D('',#12776,#10337,#10338);
#9116=AXIS2_PLACEMENT_3D('',#12785,#10343,#10344);
#9117=AXIS2_PLACEMENT_3D('',#12791,#10348,#10349);
#9118=AXIS2_PLACEMENT_3D('',#12797,#10353,#10354);
#9119=AXIS2_PLACEMENT_3D('',#12799,#10356,#10357);
#9120=AXIS2_PLACEMENT_3D('',#12808,#10362,#10363);
#9121=AXIS2_PLACEMENT_3D('',#12814,#10367,#10368);
#9122=AXIS2_PLACEMENT_3D('',#12820,#10372,#10373);
#9123=AXIS2_PLACEMENT_3D('',#12822,#10375,#10376);
#9124=AXIS2_PLACEMENT_3D('',#12831,#10381,#10382);
#9125=AXIS2_PLACEMENT_3D('',#12837,#10386,#10387);
#9126=AXIS2_PLACEMENT_3D('',#12843,#10391,#10392);
#9127=AXIS2_PLACEMENT_3D('',#12845,#10394,#10395);
#9128=AXIS2_PLACEMENT_3D('',#12854,#10400,#10401);
#9129=AXIS2_PLACEMENT_3D('',#12860,#10405,#10406);
#9130=AXIS2_PLACEMENT_3D('',#12866,#10410,#10411);
#9131=AXIS2_PLACEMENT_3D('',#12868,#10413,#10414);
#9132=AXIS2_PLACEMENT_3D('',#12877,#10419,#10420);
#9133=AXIS2_PLACEMENT_3D('',#12883,#10424,#10425);
#9134=AXIS2_PLACEMENT_3D('',#12889,#10429,#10430);
#9135=AXIS2_PLACEMENT_3D('',#12891,#10432,#10433);
#9136=AXIS2_PLACEMENT_3D('',#12900,#10438,#10439);
#9137=AXIS2_PLACEMENT_3D('',#12906,#10443,#10444);
#9138=AXIS2_PLACEMENT_3D('',#12912,#10448,#10449);
#9139=AXIS2_PLACEMENT_3D('',#12914,#10451,#10452);
#9140=AXIS2_PLACEMENT_3D('',#12923,#10457,#10458);
#9141=AXIS2_PLACEMENT_3D('',#12929,#10462,#10463);
#9142=AXIS2_PLACEMENT_3D('',#12935,#10467,#10468);
#9143=AXIS2_PLACEMENT_3D('',#12937,#10470,#10471);
#9144=AXIS2_PLACEMENT_3D('',#12976,#10505,#10506);
#9145=AXIS2_PLACEMENT_3D('',#12978,#10507,#10508);
#9146=AXIS2_PLACEMENT_3D('',#12979,#10509,#10510);
#9147=AXIS2_PLACEMENT_3D('',#12981,#10511,#10512);
#9148=AXIS2_PLACEMENT_3D('',#12983,#10514,#10515);
#9149=AXIS2_PLACEMENT_3D('',#12985,#10516,#10517);
#9150=AXIS2_PLACEMENT_3D('',#12987,#10519,#10520);
#9151=AXIS2_PLACEMENT_3D('',#12993,#10524,#10525);
#9152=AXIS2_PLACEMENT_3D('',#12997,#10528,#10529);
#9153=AXIS2_PLACEMENT_3D('',#13001,#10532,#10533);
#9154=AXIS2_PLACEMENT_3D('',#13003,#10535,#10536);
#9155=AXIS2_PLACEMENT_3D('',#13004,#10537,#10538);
#9156=AXIS2_PLACEMENT_3D('',#13005,#10539,#10540);
#9157=AXIS2_PLACEMENT_3D('',#13014,#10545,#10546);
#9158=AXIS2_PLACEMENT_3D('',#13020,#10550,#10551);
#9159=AXIS2_PLACEMENT_3D('',#13026,#10555,#10556);
#9160=AXIS2_PLACEMENT_3D('',#13029,#10559,#10560);
#9161=AXIS2_PLACEMENT_3D('',#13030,#10561,#10562);
#9162=AXIS2_PLACEMENT_3D('',#13031,#10563,#10564);
#9163=AXIS2_PLACEMENT_3D('',#13032,#10565,#10566);
#9164=AXIS2_PLACEMENT_3D('',#13041,#10571,#10572);
#9165=AXIS2_PLACEMENT_3D('',#13047,#10576,#10577);
#9166=AXIS2_PLACEMENT_3D('',#13053,#10581,#10582);
#9167=AXIS2_PLACEMENT_3D('',#13056,#10585,#10586);
#9168=AXIS2_PLACEMENT_3D('',#13057,#10587,#10588);
#9169=AXIS2_PLACEMENT_3D('',#13058,#10589,#10590);
#9170=AXIS2_PLACEMENT_3D('',#13059,#10591,#10592);
#9171=AXIS2_PLACEMENT_3D('',#13068,#10597,#10598);
#9172=AXIS2_PLACEMENT_3D('',#13074,#10602,#10603);
#9173=AXIS2_PLACEMENT_3D('',#13080,#10607,#10608);
#9174=AXIS2_PLACEMENT_3D('',#13083,#10611,#10612);
#9175=AXIS2_PLACEMENT_3D('',#13084,#10613,#10614);
#9176=AXIS2_PLACEMENT_3D('',#13085,#10615,#10616);
#9177=AXIS2_PLACEMENT_3D('',#13086,#10617,#10618);
#9178=AXIS2_PLACEMENT_3D('',#13095,#10623,#10624);
#9179=AXIS2_PLACEMENT_3D('',#13101,#10628,#10629);
#9180=AXIS2_PLACEMENT_3D('',#13107,#10633,#10634);
#9181=AXIS2_PLACEMENT_3D('',#13110,#10637,#10638);
#9182=AXIS2_PLACEMENT_3D('',#13111,#10639,#10640);
#9183=AXIS2_PLACEMENT_3D('',#13112,#10641,#10642);
#9184=AXIS2_PLACEMENT_3D('',#13113,#10643,#10644);
#9185=AXIS2_PLACEMENT_3D('',#13115,#10645,#10646);
#9186=AXIS2_PLACEMENT_3D('',#13118,#10648,#10649);
#9187=AXIS2_PLACEMENT_3D('',#13119,#10650,#10651);
#9188=AXIS2_PLACEMENT_3D('',#13121,#10652,#10653);
#9189=AXIS2_PLACEMENT_3D('',#13122,#10654,#10655);
#9190=AXIS2_PLACEMENT_3D('',#13124,#10656,#10657);
#9191=AXIS2_PLACEMENT_3D('',#13127,#10659,#10660);
#9192=AXIS2_PLACEMENT_3D('',#13128,#10661,#10662);
#9193=AXIS2_PLACEMENT_3D('',#13130,#10663,#10664);
#9194=AXIS2_PLACEMENT_3D('',#13131,#10665,#10666);
#9195=AXIS2_PLACEMENT_3D('',#13133,#10667,#10668);
#9196=AXIS2_PLACEMENT_3D('',#13136,#10670,#10671);
#9197=AXIS2_PLACEMENT_3D('',#13137,#10672,#10673);
#9198=AXIS2_PLACEMENT_3D('',#13139,#10674,#10675);
#9199=AXIS2_PLACEMENT_3D('',#13140,#10676,#10677);
#9200=AXIS2_PLACEMENT_3D('',#13142,#10678,#10679);
#9201=AXIS2_PLACEMENT_3D('',#13145,#10681,#10682);
#9202=AXIS2_PLACEMENT_3D('',#13146,#10683,#10684);
#9203=AXIS2_PLACEMENT_3D('',#13148,#10685,#10686);
#9204=AXIS2_PLACEMENT_3D('',#13149,#10687,#10688);
#9205=AXIS2_PLACEMENT_3D('',#13151,#10689,#10690);
#9206=AXIS2_PLACEMENT_3D('',#13153,#10692,#10693);
#9207=AXIS2_PLACEMENT_3D('',#13155,#10694,#10695);
#9208=AXIS2_PLACEMENT_3D('',#13157,#10697,#10698);
#9209=AXIS2_PLACEMENT_3D('',#13159,#10699,#10700);
#9210=AXIS2_PLACEMENT_3D('',#13161,#10702,#10703);
#9211=AXIS2_PLACEMENT_3D('',#13163,#10704,#10705);
#9212=AXIS2_PLACEMENT_3D('',#13165,#10707,#10708);
#9213=AXIS2_PLACEMENT_3D('',#13174,#10713,#10714);
#9214=AXIS2_PLACEMENT_3D('',#13180,#10718,#10719);
#9215=AXIS2_PLACEMENT_3D('',#13186,#10723,#10724);
#9216=AXIS2_PLACEMENT_3D('',#13192,#10728,#10729);
#9217=AXIS2_PLACEMENT_3D('',#13198,#10733,#10734);
#9218=AXIS2_PLACEMENT_3D('',#13204,#10738,#10739);
#9219=AXIS2_PLACEMENT_3D('',#13210,#10743,#10744);
#9220=AXIS2_PLACEMENT_3D('',#13216,#10748,#10749);
#9221=AXIS2_PLACEMENT_3D('',#13222,#10753,#10754);
#9222=AXIS2_PLACEMENT_3D('',#13228,#10758,#10759);
#9223=AXIS2_PLACEMENT_3D('',#13234,#10763,#10764);
#9224=AXIS2_PLACEMENT_3D('',#13237,#10767,#10768);
#9225=AXIS2_PLACEMENT_3D('',#13238,#10769,#10770);
#9226=AXIS2_PLACEMENT_3D('',#13239,#10771,#10772);
#9227=AXIS2_PLACEMENT_3D('',#13240,#10773,#10774);
#9228=AXIS2_PLACEMENT_3D('',#13249,#10779,#10780);
#9229=AXIS2_PLACEMENT_3D('',#13255,#10784,#10785);
#9230=AXIS2_PLACEMENT_3D('',#13261,#10789,#10790);
#9231=AXIS2_PLACEMENT_3D('',#13267,#10794,#10795);
#9232=AXIS2_PLACEMENT_3D('',#13273,#10799,#10800);
#9233=AXIS2_PLACEMENT_3D('',#13279,#10804,#10805);
#9234=AXIS2_PLACEMENT_3D('',#13285,#10809,#10810);
#9235=AXIS2_PLACEMENT_3D('',#13291,#10814,#10815);
#9236=AXIS2_PLACEMENT_3D('',#13297,#10819,#10820);
#9237=AXIS2_PLACEMENT_3D('',#13306,#10825,#10826);
#9238=AXIS2_PLACEMENT_3D('',#13312,#10830,#10831);
#9239=AXIS2_PLACEMENT_3D('',#13318,#10835,#10836);
#9240=AXIS2_PLACEMENT_3D('',#13324,#10840,#10841);
#9241=AXIS2_PLACEMENT_3D('',#13330,#10845,#10846);
#9242=AXIS2_PLACEMENT_3D('',#13336,#10850,#10851);
#9243=AXIS2_PLACEMENT_3D('',#13342,#10855,#10856);
#9244=AXIS2_PLACEMENT_3D('',#13348,#10860,#10861);
#9245=AXIS2_PLACEMENT_3D('',#13354,#10865,#10866);
#9246=AXIS2_PLACEMENT_3D('',#13363,#10871,#10872);
#9247=AXIS2_PLACEMENT_3D('',#13369,#10876,#10877);
#9248=AXIS2_PLACEMENT_3D('',#13375,#10881,#10882);
#9249=AXIS2_PLACEMENT_3D('',#13381,#10886,#10887);
#9250=AXIS2_PLACEMENT_3D('',#13387,#10891,#10892);
#9251=AXIS2_PLACEMENT_3D('',#13393,#10896,#10897);
#9252=AXIS2_PLACEMENT_3D('',#13399,#10901,#10902);
#9253=AXIS2_PLACEMENT_3D('',#13405,#10906,#10907);
#9254=AXIS2_PLACEMENT_3D('',#13411,#10911,#10912);
#9255=AXIS2_PLACEMENT_3D('',#13420,#10917,#10918);
#9256=AXIS2_PLACEMENT_3D('',#13426,#10922,#10923);
#9257=AXIS2_PLACEMENT_3D('',#13432,#10927,#10928);
#9258=AXIS2_PLACEMENT_3D('',#13438,#10932,#10933);
#9259=AXIS2_PLACEMENT_3D('',#13444,#10937,#10938);
#9260=AXIS2_PLACEMENT_3D('',#13450,#10942,#10943);
#9261=AXIS2_PLACEMENT_3D('',#13456,#10947,#10948);
#9262=AXIS2_PLACEMENT_3D('',#13462,#10952,#10953);
#9263=AXIS2_PLACEMENT_3D('',#13468,#10957,#10958);
#9264=AXIS2_PLACEMENT_3D('',#13470,#10959,#10960);
#9265=AXIS2_PLACEMENT_3D('',#13473,#10962,#10963);
#9266=AXIS2_PLACEMENT_3D('',#13474,#10964,#10965);
#9267=AXIS2_PLACEMENT_3D('',#13480,#10969,#10970);
#9268=AXIS2_PLACEMENT_3D('',#13486,#10974,#10975);
#9269=AXIS2_PLACEMENT_3D('',#13489,#10978,#10979);
#9270=AXIS2_PLACEMENT_3D('',#13495,#10983,#10984);
#9271=AXIS2_PLACEMENT_3D('',#13498,#10987,#10988);
#9272=AXIS2_PLACEMENT_3D('',#13504,#10992,#10993);
#9273=AXIS2_PLACEMENT_3D('',#13507,#10996,#10997);
#9274=AXIS2_PLACEMENT_3D('',#13510,#11000,#11001);
#9275=AXIS2_PLACEMENT_3D('',#13511,#11002,#11003);
#9276=AXIS2_PLACEMENT_3D('',#13512,#11004,#11005);
#9277=AXIS2_PLACEMENT_3D('',#13513,#11006,#11007);
#9278=AXIS2_PLACEMENT_3D('',#13522,#11012,#11013);
#9279=AXIS2_PLACEMENT_3D('',#13528,#11017,#11018);
#9280=AXIS2_PLACEMENT_3D('',#13535,#11022,#11023);
#9281=AXIS2_PLACEMENT_3D('',#13536,#11024,#11025);
#9282=AXIS2_PLACEMENT_3D('',#13550,#11033,#11034);
#9283=AXIS2_PLACEMENT_3D('',#13554,#11037,#11038);
#9284=AXIS2_PLACEMENT_3D('',#13558,#11041,#11042);
#9285=AXIS2_PLACEMENT_3D('',#13568,#11048,#11049);
#9286=AXIS2_PLACEMENT_3D('',#13570,#11051,#11052);
#9287=AXIS2_PLACEMENT_3D('',#13574,#11054,#11055);
#9288=AXIS2_PLACEMENT_3D('',#13576,#11057,#11058);
#9289=AXIS2_PLACEMENT_3D('',#13578,#11059,#11060);
#9290=AXIS2_PLACEMENT_3D('',#13581,#11062,#11063);
#9291=AXIS2_PLACEMENT_3D('',#13583,#11064,#11065);
#9292=AXIS2_PLACEMENT_3D('',#13584,#11066,#11067);
#9293=AXIS2_PLACEMENT_3D('',#13585,#11068,#11069);
#9294=AXIS2_PLACEMENT_3D('',#13587,#11071,#11072);
#9295=AXIS2_PLACEMENT_3D('',#13589,#11074,#11075);
#9296=AXIS2_PLACEMENT_3D('',#13591,#11077,#11078);
#9297=AXIS2_PLACEMENT_3D('',#13592,#11079,#11080);
#9298=AXIS2_PLACEMENT_3D('',#13593,#11081,#11082);
#9299=AXIS2_PLACEMENT_3D('',#13602,#11087,#11088);
#9300=AXIS2_PLACEMENT_3D('',#13608,#11092,#11093);
#9301=AXIS2_PLACEMENT_3D('',#13614,#11097,#11098);
#9302=AXIS2_PLACEMENT_3D('',#13620,#11102,#11103);
#9303=AXIS2_PLACEMENT_3D('',#13626,#11107,#11108);
#9304=AXIS2_PLACEMENT_3D('',#13629,#11111,#11112);
#9305=AXIS2_PLACEMENT_3D('',#13630,#11113,#11114);
#9306=AXIS2_PLACEMENT_3D('',#13631,#11115,#11116);
#9307=AXIS2_PLACEMENT_3D('',#13633,#11117,#11118);
#9308=AXIS2_PLACEMENT_3D('',#13634,#11119,#11120);
#9309=AXIS2_PLACEMENT_3D('',#13636,#11121,#11122);
#9310=AXIS2_PLACEMENT_3D('',#13637,#11123,#11124);
#9311=AXIS2_PLACEMENT_3D('',#13639,#11125,#11126);
#9312=AXIS2_PLACEMENT_3D('',#13641,#11128,#11129);
#9313=AXIS2_PLACEMENT_3D('',#13643,#11130,#11131);
#9314=AXIS2_PLACEMENT_3D('',#13645,#11133,#11134);
#9315=AXIS2_PLACEMENT_3D('',#13647,#11135,#11136);
#9316=AXIS2_PLACEMENT_3D('',#13649,#11138,#11139);
#9317=AXIS2_PLACEMENT_3D('',#13651,#11140,#11141);
#9318=AXIS2_PLACEMENT_3D('',#13652,#11142,#11143);
#9319=AXIS2_PLACEMENT_3D('',#13654,#11144,#11145);
#9320=AXIS2_PLACEMENT_3D('',#13656,#11147,#11148);
#9321=AXIS2_PLACEMENT_3D('',#13658,#11150,#11151);
#9322=AXIS2_PLACEMENT_3D('',#13659,#11152,#11153);
#9323=AXIS2_PLACEMENT_3D('',#13668,#11158,#11159);
#9324=AXIS2_PLACEMENT_3D('',#13674,#11163,#11164);
#9325=AXIS2_PLACEMENT_3D('',#13680,#11168,#11169);
#9326=AXIS2_PLACEMENT_3D('',#13686,#11173,#11174);
#9327=AXIS2_PLACEMENT_3D('',#13692,#11178,#11179);
#9328=AXIS2_PLACEMENT_3D('',#13695,#11182,#11183);
#9329=AXIS2_PLACEMENT_3D('',#13696,#11184,#11185);
#9330=AXIS2_PLACEMENT_3D('',#13697,#11186,#11187);
#9331=AXIS2_PLACEMENT_3D('',#13699,#11188,#11189);
#9332=AXIS2_PLACEMENT_3D('',#13700,#11190,#11191);
#9333=AXIS2_PLACEMENT_3D('',#13702,#11192,#11193);
#9334=AXIS2_PLACEMENT_3D('',#13703,#11194,#11195);
#9335=AXIS2_PLACEMENT_3D('',#13705,#11196,#11197);
#9336=AXIS2_PLACEMENT_3D('',#13707,#11199,#11200);
#9337=AXIS2_PLACEMENT_3D('',#13709,#11201,#11202);
#9338=AXIS2_PLACEMENT_3D('',#13711,#11204,#11205);
#9339=AXIS2_PLACEMENT_3D('',#13713,#11206,#11207);
#9340=AXIS2_PLACEMENT_3D('',#13715,#11209,#11210);
#9341=AXIS2_PLACEMENT_3D('',#13717,#11211,#11212);
#9342=AXIS2_PLACEMENT_3D('',#13718,#11213,#11214);
#9343=AXIS2_PLACEMENT_3D('',#13720,#11215,#11216);
#9344=AXIS2_PLACEMENT_3D('',#13722,#11218,#11219);
#9345=AXIS2_PLACEMENT_3D('',#13724,#11221,#11222);
#9346=AXIS2_PLACEMENT_3D('',#13725,#11223,#11224);
#9347=AXIS2_PLACEMENT_3D('',#13726,#11225,#11226);
#9348=AXIS2_PLACEMENT_3D('',#13728,#11227,#11228);
#9349=AXIS2_PLACEMENT_3D('',#13731,#11230,#11231);
#9350=AXIS2_PLACEMENT_3D('',#13732,#11232,#11233);
#9351=AXIS2_PLACEMENT_3D('',#13734,#11234,#11235);
#9352=AXIS2_PLACEMENT_3D('',#13737,#11237,#11238);
#9353=AXIS2_PLACEMENT_3D('',#13738,#11239,#11240);
#9354=AXIS2_PLACEMENT_3D('',#13740,#11241,#11242);
#9355=AXIS2_PLACEMENT_3D('',#13743,#11244,#11245);
#9356=AXIS2_PLACEMENT_3D('',#13744,#11246,#11247);
#9357=AXIS2_PLACEMENT_3D('',#13746,#11248,#11249);
#9358=AXIS2_PLACEMENT_3D('',#13749,#11251,#11252);
#9359=AXIS2_PLACEMENT_3D('',#13750,#11253,#11254);
#9360=AXIS2_PLACEMENT_3D('',#13752,#11255,#11256);
#9361=AXIS2_PLACEMENT_3D('',#13755,#11258,#11259);
#9362=AXIS2_PLACEMENT_3D('',#13756,#11260,#11261);
#9363=AXIS2_PLACEMENT_3D('',#13758,#11262,#11263);
#9364=AXIS2_PLACEMENT_3D('',#13761,#11265,#11266);
#9365=AXIS2_PLACEMENT_3D('',#13762,#11267,#11268);
#9366=AXIS2_PLACEMENT_3D('',#13771,#11273,#11274);
#9367=AXIS2_PLACEMENT_3D('',#13777,#11278,#11279);
#9368=AXIS2_PLACEMENT_3D('',#13783,#11283,#11284);
#9369=AXIS2_PLACEMENT_3D('',#13786,#11287,#11288);
#9370=AXIS2_PLACEMENT_3D('',#13787,#11289,#11290);
#9371=AXIS2_PLACEMENT_3D('',#13788,#11291,#11292);
#9372=AXIS2_PLACEMENT_3D('',#13789,#11293,#11294);
#9373=AXIS2_PLACEMENT_3D('',#13791,#11295,#11296);
#9374=AXIS2_PLACEMENT_3D('',#13794,#11298,#11299);
#9375=AXIS2_PLACEMENT_3D('',#13795,#11300,#11301);
#9376=AXIS2_PLACEMENT_3D('',#13804,#11306,#11307);
#9377=AXIS2_PLACEMENT_3D('',#13810,#11311,#11312);
#9378=AXIS2_PLACEMENT_3D('',#13816,#11316,#11317);
#9379=AXIS2_PLACEMENT_3D('',#13822,#11321,#11322);
#9380=AXIS2_PLACEMENT_3D('',#13828,#11326,#11327);
#9381=AXIS2_PLACEMENT_3D('',#13831,#11330,#11331);
#9382=AXIS2_PLACEMENT_3D('',#13832,#11332,#11333);
#9383=AXIS2_PLACEMENT_3D('',#13833,#11334,#11335);
#9384=AXIS2_PLACEMENT_3D('',#13834,#11336,#11337);
#9385=AXIS2_PLACEMENT_3D('',#13836,#11338,#11339);
#9386=AXIS2_PLACEMENT_3D('',#13839,#11341,#11342);
#9387=AXIS2_PLACEMENT_3D('',#13840,#11343,#11344);
#9388=AXIS2_PLACEMENT_3D('',#13842,#11345,#11346);
#9389=AXIS2_PLACEMENT_3D('',#13845,#11348,#11349);
#9390=AXIS2_PLACEMENT_3D('',#13846,#11350,#11351);
#9391=AXIS2_PLACEMENT_3D('',#13847,#11352,#11353);
#9392=AXIS2_PLACEMENT_3D('',#13848,#11354,#11355);
#9393=AXIS2_PLACEMENT_3D('',#13849,#11356,#11357);
#9394=AXIS2_PLACEMENT_3D('',#13850,#11358,#11359);
#9395=AXIS2_PLACEMENT_3D('',#13854,#11361,#11362);
#9396=AXIS2_PLACEMENT_3D('',#13855,#11363,#11364);
#9397=AXIS2_PLACEMENT_3D('',#13859,#11366,#11367);
#9398=AXIS2_PLACEMENT_3D('',#13862,#11369,#11370);
#9399=AXIS2_PLACEMENT_3D('',#13864,#11371,#11372);
#9400=AXIS2_PLACEMENT_3D('',#13866,#11374,#11375);
#9401=AXIS2_PLACEMENT_3D('',#13870,#11377,#11378);
#9402=AXIS2_PLACEMENT_3D('',#13871,#11379,#11380);
#9403=AXIS2_PLACEMENT_3D('',#13875,#11382,#11383);
#9404=AXIS2_PLACEMENT_3D('',#13878,#11385,#11386);
#9405=AXIS2_PLACEMENT_3D('',#13880,#11387,#11388);
#9406=AXIS2_PLACEMENT_3D('',#13882,#11390,#11391);
#9407=AXIS2_PLACEMENT_3D('',#13886,#11393,#11394);
#9408=AXIS2_PLACEMENT_3D('',#13887,#11395,#11396);
#9409=AXIS2_PLACEMENT_3D('',#13891,#11398,#11399);
#9410=AXIS2_PLACEMENT_3D('',#13894,#11401,#11402);
#9411=AXIS2_PLACEMENT_3D('',#13896,#11403,#11404);
#9412=AXIS2_PLACEMENT_3D('',#13898,#11406,#11407);
#9413=AXIS2_PLACEMENT_3D('',#13902,#11409,#11410);
#9414=AXIS2_PLACEMENT_3D('',#13903,#11411,#11412);
#9415=AXIS2_PLACEMENT_3D('',#13907,#11414,#11415);
#9416=AXIS2_PLACEMENT_3D('',#13910,#11417,#11418);
#9417=AXIS2_PLACEMENT_3D('',#13912,#11419,#11420);
#9418=AXIS2_PLACEMENT_3D('',#13914,#11422,#11423);
#9419=AXIS2_PLACEMENT_3D('',#13925,#11430,#11431);
#9420=AXIS2_PLACEMENT_3D('',#13936,#11438,#11439);
#9421=AXIS2_PLACEMENT_3D('',#13955,#11450,#11451);
#9422=AXIS2_PLACEMENT_3D('',#13959,#11454,#11455);
#9423=AXIS2_PLACEMENT_3D('',#13963,#11458,#11459);
#9424=AXIS2_PLACEMENT_3D('',#13967,#11462,#11463);
#9425=AXIS2_PLACEMENT_3D('',#13971,#11466,#11467);
#9426=AXIS2_PLACEMENT_3D('',#13973,#11469,#11470);
#9427=AXIS2_PLACEMENT_3D('',#13977,#11473,#11474);
#9428=AXIS2_PLACEMENT_3D('',#13981,#11477,#11478);
#9429=AXIS2_PLACEMENT_3D('',#13985,#11481,#11482);
#9430=AXIS2_PLACEMENT_3D('',#13989,#11485,#11486);
#9431=AXIS2_PLACEMENT_3D('',#13991,#11488,#11489);
#9432=AXIS2_PLACEMENT_3D('',#13992,#11490,#11491);
#9433=AXIS2_PLACEMENT_3D('',#13993,#11492,#11493);
#9434=AXIS2_PLACEMENT_3D('',#14002,#11498,#11499);
#9435=AXIS2_PLACEMENT_3D('',#14008,#11503,#11504);
#9436=AXIS2_PLACEMENT_3D('',#14014,#11508,#11509);
#9437=AXIS2_PLACEMENT_3D('',#14020,#11513,#11514);
#9438=AXIS2_PLACEMENT_3D('',#14026,#11518,#11519);
#9439=AXIS2_PLACEMENT_3D('',#14032,#11523,#11524);
#9440=AXIS2_PLACEMENT_3D('',#14038,#11528,#11529);
#9441=AXIS2_PLACEMENT_3D('',#14041,#11532,#11533);
#9442=AXIS2_PLACEMENT_3D('',#14042,#11534,#11535);
#9443=AXIS2_PLACEMENT_3D('',#14043,#11536,#11537);
#9444=AXIS2_PLACEMENT_3D('',#14044,#11538,#11539);
#9445=AXIS2_PLACEMENT_3D('',#14053,#11544,#11545);
#9446=AXIS2_PLACEMENT_3D('',#14059,#11549,#11550);
#9447=AXIS2_PLACEMENT_3D('',#14065,#11554,#11555);
#9448=AXIS2_PLACEMENT_3D('',#14071,#11559,#11560);
#9449=AXIS2_PLACEMENT_3D('',#14077,#11564,#11565);
#9450=AXIS2_PLACEMENT_3D('',#14083,#11569,#11570);
#9451=AXIS2_PLACEMENT_3D('',#14089,#11574,#11575);
#9452=AXIS2_PLACEMENT_3D('',#14092,#11578,#11579);
#9453=AXIS2_PLACEMENT_3D('',#14093,#11580,#11581);
#9454=AXIS2_PLACEMENT_3D('',#14094,#11582,#11583);
#9455=AXIS2_PLACEMENT_3D('',#14095,#11584,#11585);
#9456=AXIS2_PLACEMENT_3D('',#14096,#11586,#11587);
#9457=AXIS2_PLACEMENT_3D('',#14097,#11588,#11589);
#9458=AXIS2_PLACEMENT_3D('',#14098,#11590,#11591);
#9459=AXIS2_PLACEMENT_3D('',#14100,#11592,#11593);
#9460=AXIS2_PLACEMENT_3D('',#14103,#11595,#11596);
#9461=AXIS2_PLACEMENT_3D('',#14104,#11597,#11598);
#9462=AXIS2_PLACEMENT_3D('',#14107,#11600,#11601);
#9463=AXIS2_PLACEMENT_3D('',#14108,#11602,#11603);
#9464=AXIS2_PLACEMENT_3D('',#14110,#11604,#11605);
#9465=AXIS2_PLACEMENT_3D('',#14111,#11606,#11607);
#9466=AXIS2_PLACEMENT_3D('',#14114,#11609,#11610);
#9467=AXIS2_PLACEMENT_3D('',#14115,#11611,#11612);
#9468=AXIS2_PLACEMENT_3D('',#14116,#11613,#11614);
#9469=AXIS2_PLACEMENT_3D('',#14117,#11615,#11616);
#9470=AXIS2_PLACEMENT_3D('',#14119,#11617,#11618);
#9471=AXIS2_PLACEMENT_3D('',#14120,#11619,#11620);
#9472=AXIS2_PLACEMENT_3D('',#14122,#11621,#11622);
#9473=AXIS2_PLACEMENT_3D('',#14124,#11624,#11625);
#9474=AXIS2_PLACEMENT_3D('',#14126,#11626,#11627);
#9475=AXIS2_PLACEMENT_3D('',#14128,#11629,#11630);
#9476=AXIS2_PLACEMENT_3D('',#14130,#11631,#11632);
#9477=AXIS2_PLACEMENT_3D('',#14132,#11634,#11635);
#9478=AXIS2_PLACEMENT_3D('',#14134,#11636,#11637);
#9479=AXIS2_PLACEMENT_3D('',#14135,#11638,#11639);
#9480=AXIS2_PLACEMENT_3D('',#14137,#11640,#11641);
#9481=AXIS2_PLACEMENT_3D('',#14139,#11643,#11644);
#9482=AXIS2_PLACEMENT_3D('',#14141,#11645,#11646);
#9483=AXIS2_PLACEMENT_3D('',#14143,#11648,#11649);
#9484=AXIS2_PLACEMENT_3D('',#14145,#11650,#11651);
#9485=AXIS2_PLACEMENT_3D('',#14147,#11653,#11654);
#9486=AXIS2_PLACEMENT_3D('',#14148,#11655,#11656);
#9487=AXIS2_PLACEMENT_3D('',#14157,#11661,#11662);
#9488=AXIS2_PLACEMENT_3D('',#14163,#11666,#11667);
#9489=AXIS2_PLACEMENT_3D('',#14169,#11671,#11672);
#9490=AXIS2_PLACEMENT_3D('',#14175,#11676,#11677);
#9491=AXIS2_PLACEMENT_3D('',#14181,#11681,#11682);
#9492=AXIS2_PLACEMENT_3D('',#14184,#11685,#11686);
#9493=AXIS2_PLACEMENT_3D('',#14185,#11687,#11688);
#9494=AXIS2_PLACEMENT_3D('',#14186,#11689,#11690);
#9495=AXIS2_PLACEMENT_3D('',#14187,#11691,#11692);
#9496=AXIS2_PLACEMENT_3D('',#14189,#11693,#11694);
#9497=AXIS2_PLACEMENT_3D('',#14192,#11696,#11697);
#9498=AXIS2_PLACEMENT_3D('',#14193,#11698,#11699);
#9499=AXIS2_PLACEMENT_3D('',#14196,#11701,#11702);
#9500=AXIS2_PLACEMENT_3D('',#14197,#11703,#11704);
#9501=AXIS2_PLACEMENT_3D('',#14199,#11705,#11706);
#9502=AXIS2_PLACEMENT_3D('',#14200,#11707,#11708);
#9503=AXIS2_PLACEMENT_3D('',#14203,#11710,#11711);
#9504=AXIS2_PLACEMENT_3D('',#14204,#11712,#11713);
#9505=AXIS2_PLACEMENT_3D('',#14205,#11714,#11715);
#9506=AXIS2_PLACEMENT_3D('',#14206,#11716,#11717);
#9507=AXIS2_PLACEMENT_3D('',#14208,#11718,#11719);
#9508=AXIS2_PLACEMENT_3D('',#14209,#11720,#11721);
#9509=AXIS2_PLACEMENT_3D('',#14211,#11722,#11723);
#9510=AXIS2_PLACEMENT_3D('',#14213,#11725,#11726);
#9511=AXIS2_PLACEMENT_3D('',#14215,#11727,#11728);
#9512=AXIS2_PLACEMENT_3D('',#14217,#11730,#11731);
#9513=AXIS2_PLACEMENT_3D('',#14219,#11732,#11733);
#9514=AXIS2_PLACEMENT_3D('',#14221,#11735,#11736);
#9515=AXIS2_PLACEMENT_3D('',#14223,#11737,#11738);
#9516=AXIS2_PLACEMENT_3D('',#14224,#11739,#11740);
#9517=AXIS2_PLACEMENT_3D('',#14226,#11741,#11742);
#9518=AXIS2_PLACEMENT_3D('',#14228,#11744,#11745);
#9519=AXIS2_PLACEMENT_3D('',#14230,#11746,#11747);
#9520=AXIS2_PLACEMENT_3D('',#14232,#11749,#11750);
#9521=AXIS2_PLACEMENT_3D('',#14234,#11751,#11752);
#9522=AXIS2_PLACEMENT_3D('',#14236,#11754,#11755);
#9523=AXIS2_PLACEMENT_3D('',#14237,#11756,#11757);
#9524=AXIS2_PLACEMENT_3D('',#14246,#11762,#11763);
#9525=AXIS2_PLACEMENT_3D('',#14252,#11767,#11768);
#9526=AXIS2_PLACEMENT_3D('',#14258,#11772,#11773);
#9527=AXIS2_PLACEMENT_3D('',#14264,#11777,#11778);
#9528=AXIS2_PLACEMENT_3D('',#14270,#11782,#11783);
#9529=AXIS2_PLACEMENT_3D('',#14273,#11786,#11787);
#9530=AXIS2_PLACEMENT_3D('',#14274,#11788,#11789);
#9531=AXIS2_PLACEMENT_3D('',#14275,#11790,#11791);
#9532=AXIS2_PLACEMENT_3D('',#14276,#11792,#11793);
#9533=AXIS2_PLACEMENT_3D('',#14277,#11794,#11795);
#9534=AXIS2_PLACEMENT_3D('',#14278,#11796,#11797);
#9535=AXIS2_PLACEMENT_3D('',#14279,#11798,#11799);
#9536=AXIS2_PLACEMENT_3D('',#14280,#11800,#11801);
#9537=AXIS2_PLACEMENT_3D('',#14281,#11802,#11803);
#9538=AXIS2_PLACEMENT_3D('',#14282,#11804,#11805);
#9539=AXIS2_PLACEMENT_3D('',#14283,#11806,#11807);
#9540=AXIS2_PLACEMENT_3D('',#14284,#11808,#11809);
#9541=AXIS2_PLACEMENT_3D('',#14285,#11810,#11811);
#9542=AXIS2_PLACEMENT_3D('',#14286,#11812,#11813);
#9543=AXIS2_PLACEMENT_3D('',#14287,#11814,#11815);
#9544=AXIS2_PLACEMENT_3D('',#14288,#11816,#11817);
#9545=AXIS2_PLACEMENT_3D('',#14289,#11818,#11819);
#9546=AXIS2_PLACEMENT_3D('',#14290,#11820,#11821);
#9547=AXIS2_PLACEMENT_3D('',#14291,#11822,#11823);
#9548=AXIS2_PLACEMENT_3D('',#14292,#11824,#11825);
#9549=AXIS2_PLACEMENT_3D('',#14293,#11826,#11827);
#9550=AXIS2_PLACEMENT_3D('',#14294,#11828,#11829);
#9551=AXIS2_PLACEMENT_3D('',#14295,#11830,#11831);
#9552=AXIS2_PLACEMENT_3D('',#14296,#11832,#11833);
#9553=AXIS2_PLACEMENT_3D('',#14297,#11834,#11835);
#9554=AXIS2_PLACEMENT_3D('',#14298,#11836,#11837);
#9555=AXIS2_PLACEMENT_3D('',#14299,#11838,#11839);
#9556=AXIS2_PLACEMENT_3D('',#14300,#11840,#11841);
#9557=AXIS2_PLACEMENT_3D('',#14301,#11842,#11843);
#9558=AXIS2_PLACEMENT_3D('',#14302,#11844,#11845);
#9559=AXIS2_PLACEMENT_3D('',#14303,#11846,#11847);
#9560=AXIS2_PLACEMENT_3D('',#14304,#11848,#11849);
#9561=AXIS2_PLACEMENT_3D('',#14305,#11850,#11851);
#9562=AXIS2_PLACEMENT_3D('',#14306,#11852,#11853);
#9563=AXIS2_PLACEMENT_3D('',#14307,#11854,#11855);
#9564=AXIS2_PLACEMENT_3D('',#14308,#11856,#11857);
#9565=AXIS2_PLACEMENT_3D('',#14309,#11858,#11859);
#9566=AXIS2_PLACEMENT_3D('',#14310,#11860,#11861);
#9567=AXIS2_PLACEMENT_3D('',#14311,#11862,#11863);
#9568=AXIS2_PLACEMENT_3D('',#14312,#11864,#11865);
#9569=AXIS2_PLACEMENT_3D('',#14313,#11866,#11867);
#9570=AXIS2_PLACEMENT_3D('',#14315,#11868,#11869);
#9571=AXIS2_PLACEMENT_3D('',#14318,#11871,#11872);
#9572=AXIS2_PLACEMENT_3D('',#14319,#11873,#11874);
#9573=AXIS2_PLACEMENT_3D('',#14321,#11875,#11876);
#9574=AXIS2_PLACEMENT_3D('',#14324,#11878,#11879);
#9575=AXIS2_PLACEMENT_3D('',#14325,#11880,#11881);
#9576=AXIS2_PLACEMENT_3D('',#14326,#11882,#11883);
#9577=AXIS2_PLACEMENT_3D('',#14327,#11884,#11885);
#9578=AXIS2_PLACEMENT_3D('',#14328,#11886,#11887);
#9579=AXIS2_PLACEMENT_3D('',#14330,#11888,#11889);
#9580=AXIS2_PLACEMENT_3D('',#14331,#11890,#11891);
#9581=AXIS2_PLACEMENT_3D('',#14333,#11892,#11893);
#9582=AXIS2_PLACEMENT_3D('',#14335,#11895,#11896);
#9583=AXIS2_PLACEMENT_3D('',#14337,#11897,#11898);
#9584=AXIS2_PLACEMENT_3D('',#14339,#11900,#11901);
#9585=AXIS2_PLACEMENT_3D('',#14341,#11902,#11903);
#9586=AXIS2_PLACEMENT_3D('',#14343,#11905,#11906);
#9587=AXIS2_PLACEMENT_3D('',#14345,#11907,#11908);
#9588=AXIS2_PLACEMENT_3D('',#14346,#11909,#11910);
#9589=AXIS2_PLACEMENT_3D('',#14348,#11911,#11912);
#9590=AXIS2_PLACEMENT_3D('',#14350,#11914,#11915);
#9591=AXIS2_PLACEMENT_3D('',#14352,#11916,#11917);
#9592=AXIS2_PLACEMENT_3D('',#14354,#11919,#11920);
#9593=AXIS2_PLACEMENT_3D('',#14356,#11921,#11922);
#9594=AXIS2_PLACEMENT_3D('',#14358,#11924,#11925);
#9595=AXIS2_PLACEMENT_3D('',#14359,#11926,#11927);
#9596=AXIS2_PLACEMENT_3D('',#14368,#11932,#11933);
#9597=AXIS2_PLACEMENT_3D('',#14374,#11937,#11938);
#9598=AXIS2_PLACEMENT_3D('',#14380,#11942,#11943);
#9599=AXIS2_PLACEMENT_3D('',#14386,#11947,#11948);
#9600=AXIS2_PLACEMENT_3D('',#14392,#11952,#11953);
#9601=AXIS2_PLACEMENT_3D('',#14395,#11956,#11957);
#9602=AXIS2_PLACEMENT_3D('',#14396,#11958,#11959);
#9603=AXIS2_PLACEMENT_3D('',#14397,#11960,#11961);
#9604=AXIS2_PLACEMENT_3D('',#14398,#11962,#11963);
#9605=AXIS2_PLACEMENT_3D('',#14399,#11964,#11965);
#9606=AXIS2_PLACEMENT_3D('',#14400,#11966,#11967);
#9607=AXIS2_PLACEMENT_3D('',#14401,#11968,#11969);
#9608=AXIS2_PLACEMENT_3D('',#14402,#11970,#11971);
#9609=AXIS2_PLACEMENT_3D('',#14403,#11972,#11973);
#9610=AXIS2_PLACEMENT_3D('',#14404,#11974,#11975);
#9611=AXIS2_PLACEMENT_3D('',#14405,#11976,#11977);
#9612=AXIS2_PLACEMENT_3D('',#14406,#11978,#11979);
#9613=AXIS2_PLACEMENT_3D('',#14407,#11980,#11981);
#9614=AXIS2_PLACEMENT_3D('',#14408,#11982,#11983);
#9615=AXIS2_PLACEMENT_3D('',#14409,#11984,#11985);
#9616=AXIS2_PLACEMENT_3D('',#14410,#11986,#11987);
#9617=AXIS2_PLACEMENT_3D('',#14411,#11988,#11989);
#9618=AXIS2_PLACEMENT_3D('',#14412,#11990,#11991);
#9619=AXIS2_PLACEMENT_3D('',#14413,#11992,#11993);
#9620=AXIS2_PLACEMENT_3D('',#14414,#11994,#11995);
#9621=DIRECTION('axis',(0.,0.,1.));
#9622=DIRECTION('refdir',(1.,0.,0.));
#9623=DIRECTION('axis',(0.,0.,1.));
#9624=DIRECTION('refdir',(1.,0.,0.));
#9625=DIRECTION('axis',(0.,0.,1.));
#9626=DIRECTION('refdir',(1.,0.,0.));
#9627=DIRECTION('center_axis',(0.,0.,1.));
#9628=DIRECTION('ref_axis',(1.,0.,0.));
#9629=DIRECTION('center_axis',(0.,0.,1.));
#9630=DIRECTION('ref_axis',(1.,0.,0.));
#9631=DIRECTION('',(0.,0.,1.));
#9632=DIRECTION('center_axis',(0.,0.,-1.));
#9633=DIRECTION('ref_axis',(1.,0.,0.));
#9634=DIRECTION('center_axis',(0.,0.,1.));
#9635=DIRECTION('ref_axis',(1.,0.,0.));
#9636=DIRECTION('center_axis',(0.,0.,1.));
#9637=DIRECTION('ref_axis',(1.,0.,0.));
#9638=DIRECTION('',(0.,0.,1.));
#9639=DIRECTION('center_axis',(0.,0.,-1.));
#9640=DIRECTION('ref_axis',(1.,0.,0.));
#9641=DIRECTION('center_axis',(0.,0.,1.));
#9642=DIRECTION('ref_axis',(1.,0.,0.));
#9643=DIRECTION('center_axis',(0.,0.,1.));
#9644=DIRECTION('ref_axis',(1.,0.,0.));
#9645=DIRECTION('',(0.,0.,1.));
#9646=DIRECTION('center_axis',(0.,0.,-1.));
#9647=DIRECTION('ref_axis',(1.,0.,0.));
#9648=DIRECTION('center_axis',(0.,0.,1.));
#9649=DIRECTION('ref_axis',(1.,0.,0.));
#9650=DIRECTION('center_axis',(0.,0.,1.));
#9651=DIRECTION('ref_axis',(1.,0.,0.));
#9652=DIRECTION('',(0.,0.,1.));
#9653=DIRECTION('center_axis',(0.,0.,-1.));
#9654=DIRECTION('ref_axis',(1.,0.,0.));
#9655=DIRECTION('center_axis',(0.,0.,1.));
#9656=DIRECTION('ref_axis',(1.,0.,0.));
#9657=DIRECTION('center_axis',(0.,0.,1.));
#9658=DIRECTION('ref_axis',(1.,0.,0.));
#9659=DIRECTION('',(0.,0.,1.));
#9660=DIRECTION('center_axis',(0.,0.,-1.));
#9661=DIRECTION('ref_axis',(1.,0.,0.));
#9662=DIRECTION('center_axis',(0.,0.,1.));
#9663=DIRECTION('ref_axis',(1.,0.,0.));
#9664=DIRECTION('center_axis',(0.,0.,1.));
#9665=DIRECTION('ref_axis',(1.,0.,0.));
#9666=DIRECTION('',(0.,0.,1.));
#9667=DIRECTION('center_axis',(0.,0.,-1.));
#9668=DIRECTION('ref_axis',(1.,0.,0.));
#9669=DIRECTION('center_axis',(0.,0.,1.));
#9670=DIRECTION('ref_axis',(1.,0.,0.));
#9671=DIRECTION('center_axis',(0.,0.,1.));
#9672=DIRECTION('ref_axis',(1.,0.,0.));
#9673=DIRECTION('',(0.,0.,1.));
#9674=DIRECTION('center_axis',(0.,0.,-1.));
#9675=DIRECTION('ref_axis',(1.,0.,0.));
#9676=DIRECTION('center_axis',(0.,0.,1.));
#9677=DIRECTION('ref_axis',(1.,0.,0.));
#9678=DIRECTION('center_axis',(0.,0.,1.));
#9679=DIRECTION('ref_axis',(1.,0.,0.));
#9680=DIRECTION('',(0.,0.,1.));
#9681=DIRECTION('center_axis',(0.,0.,-1.));
#9682=DIRECTION('ref_axis',(1.,0.,0.));
#9683=DIRECTION('center_axis',(0.,0.,1.));
#9684=DIRECTION('ref_axis',(1.,0.,0.));
#9685=DIRECTION('center_axis',(0.,0.,1.));
#9686=DIRECTION('ref_axis',(1.,0.,0.));
#9687=DIRECTION('',(0.,0.,1.));
#9688=DIRECTION('center_axis',(0.,0.,-1.));
#9689=DIRECTION('ref_axis',(1.,0.,0.));
#9690=DIRECTION('center_axis',(0.,0.,1.));
#9691=DIRECTION('ref_axis',(1.,0.,0.));
#9692=DIRECTION('center_axis',(0.,0.,1.));
#9693=DIRECTION('ref_axis',(1.,0.,0.));
#9694=DIRECTION('',(0.,0.,1.));
#9695=DIRECTION('center_axis',(0.,0.,-1.));
#9696=DIRECTION('ref_axis',(1.,0.,0.));
#9697=DIRECTION('center_axis',(0.,0.,1.));
#9698=DIRECTION('ref_axis',(1.,0.,0.));
#9699=DIRECTION('center_axis',(0.,0.,1.));
#9700=DIRECTION('ref_axis',(1.,0.,0.));
#9701=DIRECTION('',(0.,0.,1.));
#9702=DIRECTION('center_axis',(0.,0.,-1.));
#9703=DIRECTION('ref_axis',(1.,0.,0.));
#9704=DIRECTION('center_axis',(0.,0.,1.));
#9705=DIRECTION('ref_axis',(1.,0.,0.));
#9706=DIRECTION('center_axis',(0.,0.,1.));
#9707=DIRECTION('ref_axis',(1.,0.,0.));
#9708=DIRECTION('',(0.,0.,1.));
#9709=DIRECTION('center_axis',(0.,0.,-1.));
#9710=DIRECTION('ref_axis',(1.,0.,0.));
#9711=DIRECTION('center_axis',(0.,0.,1.));
#9712=DIRECTION('ref_axis',(1.,0.,0.));
#9713=DIRECTION('center_axis',(0.,0.,1.));
#9714=DIRECTION('ref_axis',(1.,0.,0.));
#9715=DIRECTION('',(0.,0.,1.));
#9716=DIRECTION('center_axis',(0.,0.,-1.));
#9717=DIRECTION('ref_axis',(1.,0.,0.));
#9718=DIRECTION('center_axis',(0.,0.,1.));
#9719=DIRECTION('ref_axis',(1.,0.,0.));
#9720=DIRECTION('center_axis',(0.,0.,1.));
#9721=DIRECTION('ref_axis',(1.,0.,0.));
#9722=DIRECTION('',(0.,0.,1.));
#9723=DIRECTION('center_axis',(0.,0.,-1.));
#9724=DIRECTION('ref_axis',(1.,0.,0.));
#9725=DIRECTION('center_axis',(0.,1.,0.));
#9726=DIRECTION('ref_axis',(-1.,0.,0.));
#9727=DIRECTION('',(-1.,0.,0.));
#9728=DIRECTION('',(0.,0.,1.));
#9729=DIRECTION('',(-1.,0.,0.));
#9730=DIRECTION('',(0.,0.,1.));
#9731=DIRECTION('center_axis',(1.,0.,0.));
#9732=DIRECTION('ref_axis',(0.,1.,0.));
#9733=DIRECTION('',(0.,1.,0.));
#9734=DIRECTION('',(0.,1.,0.));
#9735=DIRECTION('',(0.,0.,1.));
#9736=DIRECTION('center_axis',(0.,-1.,0.));
#9737=DIRECTION('ref_axis',(1.,0.,0.));
#9738=DIRECTION('',(1.,0.,0.));
#9739=DIRECTION('',(1.,0.,0.));
#9740=DIRECTION('',(0.,0.,1.));
#9741=DIRECTION('center_axis',(-1.,0.,0.));
#9742=DIRECTION('ref_axis',(0.,-1.,0.));
#9743=DIRECTION('',(0.,-1.,0.));
#9744=DIRECTION('',(0.,-1.,0.));
#9745=DIRECTION('center_axis',(0.,0.,1.));
#9746=DIRECTION('ref_axis',(1.,0.,0.));
#9747=DIRECTION('center_axis',(0.,0.,1.));
#9748=DIRECTION('ref_axis',(1.,0.,0.));
#9749=DIRECTION('axis',(0.,0.,1.));
#9750=DIRECTION('refdir',(1.,0.,0.));
#9751=DIRECTION('center_axis',(0.,0.,1.));
#9752=DIRECTION('ref_axis',(1.,0.,0.));
#9753=DIRECTION('center_axis',(0.,0.,1.));
#9754=DIRECTION('ref_axis',(1.,0.,0.));
#9755=DIRECTION('',(0.,0.,1.));
#9756=DIRECTION('center_axis',(0.,0.,-1.));
#9757=DIRECTION('ref_axis',(1.,0.,0.));
#9758=DIRECTION('center_axis',(0.,0.,1.));
#9759=DIRECTION('ref_axis',(1.,0.,0.));
#9760=DIRECTION('center_axis',(0.,0.,1.));
#9761=DIRECTION('ref_axis',(1.,0.,0.));
#9762=DIRECTION('center_axis',(0.,0.,1.));
#9763=DIRECTION('ref_axis',(1.,0.,0.));
#9764=DIRECTION('center_axis',(0.,0.,1.));
#9765=DIRECTION('ref_axis',(1.,0.,0.));
#9766=DIRECTION('',(0.,0.,1.));
#9767=DIRECTION('center_axis',(0.,0.,-1.));
#9768=DIRECTION('ref_axis',(1.,0.,0.));
#9769=DIRECTION('center_axis',(0.,0.,1.));
#9770=DIRECTION('ref_axis',(1.,0.,0.));
#9771=DIRECTION('center_axis',(0.,0.,1.));
#9772=DIRECTION('ref_axis',(1.,0.,0.));
#9773=DIRECTION('center_axis',(0.,0.,1.));
#9774=DIRECTION('ref_axis',(1.,0.,0.));
#9775=DIRECTION('center_axis',(0.,0.,1.));
#9776=DIRECTION('ref_axis',(1.,0.,0.));
#9777=DIRECTION('',(0.,0.,1.));
#9778=DIRECTION('center_axis',(0.,0.,1.));
#9779=DIRECTION('ref_axis',(1.,0.,0.));
#9780=DIRECTION('center_axis',(0.,0.,1.));
#9781=DIRECTION('ref_axis',(1.,0.,0.));
#9782=DIRECTION('',(0.,0.,1.));
#9783=DIRECTION('center_axis',(0.,1.,0.));
#9784=DIRECTION('ref_axis',(-1.,0.,0.));
#9785=DIRECTION('',(-1.,0.,0.));
#9786=DIRECTION('',(0.,0.,1.));
#9787=DIRECTION('',(-1.,0.,0.));
#9788=DIRECTION('',(0.,0.,1.));
#9789=DIRECTION('center_axis',(1.,0.,0.));
#9790=DIRECTION('ref_axis',(0.,1.,0.));
#9791=DIRECTION('',(0.,1.,0.));
#9792=DIRECTION('',(0.,1.,0.));
#9793=DIRECTION('',(0.,0.,1.));
#9794=DIRECTION('center_axis',(0.,-1.,0.));
#9795=DIRECTION('ref_axis',(1.,0.,0.));
#9796=DIRECTION('',(1.,0.,0.));
#9797=DIRECTION('',(1.,0.,0.));
#9798=DIRECTION('',(0.,0.,1.));
#9799=DIRECTION('center_axis',(-1.,0.,0.));
#9800=DIRECTION('ref_axis',(0.,-1.,0.));
#9801=DIRECTION('',(0.,-1.,0.));
#9802=DIRECTION('',(0.,-1.,0.));
#9803=DIRECTION('center_axis',(0.,0.,1.));
#9804=DIRECTION('ref_axis',(1.,0.,0.));
#9805=DIRECTION('center_axis',(0.,0.,1.));
#9806=DIRECTION('ref_axis',(1.,0.,0.));
#9807=DIRECTION('axis',(0.,0.,1.));
#9808=DIRECTION('refdir',(1.,0.,0.));
#9809=DIRECTION('center_axis',(0.,1.,0.));
#9810=DIRECTION('ref_axis',(-1.,0.,0.));
#9811=DIRECTION('',(-1.,0.,0.));
#9812=DIRECTION('',(0.,0.,1.));
#9813=DIRECTION('',(-1.,0.,0.));
#9814=DIRECTION('',(0.,0.,1.));
#9815=DIRECTION('center_axis',(1.,0.,0.));
#9816=DIRECTION('ref_axis',(0.,1.,0.));
#9817=DIRECTION('',(0.,1.,0.));
#9818=DIRECTION('',(0.,1.,0.));
#9819=DIRECTION('',(0.,0.,1.));
#9820=DIRECTION('center_axis',(0.,-1.,0.));
#9821=DIRECTION('ref_axis',(1.,0.,0.));
#9822=DIRECTION('',(1.,0.,0.));
#9823=DIRECTION('',(1.,0.,0.));
#9824=DIRECTION('',(0.,0.,1.));
#9825=DIRECTION('center_axis',(-1.,0.,0.));
#9826=DIRECTION('ref_axis',(0.,-1.,0.));
#9827=DIRECTION('',(0.,-1.,0.));
#9828=DIRECTION('',(0.,-1.,0.));
#9829=DIRECTION('center_axis',(0.,0.,1.));
#9830=DIRECTION('ref_axis',(1.,0.,0.));
#9831=DIRECTION('center_axis',(0.,0.,1.));
#9832=DIRECTION('ref_axis',(1.,0.,0.));
#9833=DIRECTION('axis',(0.,0.,1.));
#9834=DIRECTION('refdir',(1.,0.,0.));
#9835=DIRECTION('center_axis',(0.,0.,1.));
#9836=DIRECTION('ref_axis',(1.,0.,0.));
#9837=DIRECTION('center_axis',(0.,0.,1.));
#9838=DIRECTION('ref_axis',(1.,0.,0.));
#9839=DIRECTION('',(0.,0.,1.));
#9840=DIRECTION('center_axis',(0.,0.,-1.));
#9841=DIRECTION('ref_axis',(1.,0.,0.));
#9842=DIRECTION('center_axis',(0.,0.,1.));
#9843=DIRECTION('ref_axis',(1.,0.,0.));
#9844=DIRECTION('center_axis',(0.,0.,1.));
#9845=DIRECTION('ref_axis',(1.,0.,0.));
#9846=DIRECTION('center_axis',(0.,0.,1.));
#9847=DIRECTION('ref_axis',(1.,0.,0.));
#9848=DIRECTION('center_axis',(0.,0.,1.));
#9849=DIRECTION('ref_axis',(1.,0.,0.));
#9850=DIRECTION('',(0.,0.,1.));
#9851=DIRECTION('center_axis',(0.,0.,-1.));
#9852=DIRECTION('ref_axis',(1.,0.,0.));
#9853=DIRECTION('center_axis',(0.,0.,1.));
#9854=DIRECTION('ref_axis',(1.,0.,0.));
#9855=DIRECTION('center_axis',(0.,0.,1.));
#9856=DIRECTION('ref_axis',(1.,0.,0.));
#9857=DIRECTION('center_axis',(0.,0.,1.));
#9858=DIRECTION('ref_axis',(1.,0.,0.));
#9859=DIRECTION('center_axis',(0.,0.,1.));
#9860=DIRECTION('ref_axis',(1.,0.,0.));
#9861=DIRECTION('',(0.,0.,1.));
#9862=DIRECTION('center_axis',(0.,0.,1.));
#9863=DIRECTION('ref_axis',(1.,0.,0.));
#9864=DIRECTION('center_axis',(0.,0.,1.));
#9865=DIRECTION('ref_axis',(1.,0.,0.));
#9866=DIRECTION('',(0.,0.,1.));
#9867=DIRECTION('center_axis',(0.,1.,0.));
#9868=DIRECTION('ref_axis',(-1.,0.,0.));
#9869=DIRECTION('',(-1.,0.,0.));
#9870=DIRECTION('',(0.,0.,1.));
#9871=DIRECTION('',(-1.,0.,0.));
#9872=DIRECTION('',(0.,0.,1.));
#9873=DIRECTION('center_axis',(1.,0.,0.));
#9874=DIRECTION('ref_axis',(0.,1.,0.));
#9875=DIRECTION('',(0.,1.,0.));
#9876=DIRECTION('',(0.,1.,0.));
#9877=DIRECTION('',(0.,0.,1.));
#9878=DIRECTION('center_axis',(0.,-1.,0.));
#9879=DIRECTION('ref_axis',(1.,0.,0.));
#9880=DIRECTION('',(1.,0.,0.));
#9881=DIRECTION('',(1.,0.,0.));
#9882=DIRECTION('',(0.,0.,1.));
#9883=DIRECTION('center_axis',(-1.,0.,0.));
#9884=DIRECTION('ref_axis',(0.,-1.,0.));
#9885=DIRECTION('',(0.,-1.,0.));
#9886=DIRECTION('',(0.,-1.,0.));
#9887=DIRECTION('center_axis',(0.,0.,1.));
#9888=DIRECTION('ref_axis',(1.,0.,0.));
#9889=DIRECTION('center_axis',(0.,0.,1.));
#9890=DIRECTION('ref_axis',(1.,0.,0.));
#9891=DIRECTION('axis',(0.,0.,1.));
#9892=DIRECTION('refdir',(1.,0.,0.));
#9893=DIRECTION('center_axis',(0.,1.,0.));
#9894=DIRECTION('ref_axis',(-1.,0.,0.));
#9895=DIRECTION('',(-1.,0.,0.));
#9896=DIRECTION('',(0.,0.,1.));
#9897=DIRECTION('',(-1.,0.,0.));
#9898=DIRECTION('',(0.,0.,1.));
#9899=DIRECTION('center_axis',(1.,0.,0.));
#9900=DIRECTION('ref_axis',(0.,1.,0.));
#9901=DIRECTION('',(0.,1.,0.));
#9902=DIRECTION('',(0.,1.,0.));
#9903=DIRECTION('',(0.,0.,1.));
#9904=DIRECTION('center_axis',(0.,-1.,0.));
#9905=DIRECTION('ref_axis',(1.,0.,0.));
#9906=DIRECTION('',(1.,0.,0.));
#9907=DIRECTION('',(1.,0.,0.));
#9908=DIRECTION('',(0.,0.,1.));
#9909=DIRECTION('center_axis',(-1.,0.,0.));
#9910=DIRECTION('ref_axis',(0.,-1.,0.));
#9911=DIRECTION('',(0.,-1.,0.));
#9912=DIRECTION('',(0.,-1.,0.));
#9913=DIRECTION('center_axis',(0.,0.,1.));
#9914=DIRECTION('ref_axis',(1.,0.,0.));
#9915=DIRECTION('center_axis',(0.,0.,1.));
#9916=DIRECTION('ref_axis',(1.,0.,0.));
#9917=DIRECTION('axis',(0.,0.,1.));
#9918=DIRECTION('refdir',(1.,0.,0.));
#9919=DIRECTION('center_axis',(0.,1.,0.));
#9920=DIRECTION('ref_axis',(-1.,0.,0.));
#9921=DIRECTION('',(-1.,0.,0.));
#9922=DIRECTION('',(0.,0.,1.));
#9923=DIRECTION('',(1.,0.,0.));
#9924=DIRECTION('',(0.,0.,1.));
#9925=DIRECTION('center_axis',(1.,0.,0.));
#9926=DIRECTION('ref_axis',(0.,1.,0.));
#9927=DIRECTION('',(0.,1.,0.));
#9928=DIRECTION('',(0.,0.,-1.));
#9929=DIRECTION('',(0.,-1.,0.));
#9930=DIRECTION('center_axis',(-1.,0.,0.));
#9931=DIRECTION('ref_axis',(0.,-1.,0.));
#9932=DIRECTION('',(0.,-1.,0.));
#9933=DIRECTION('',(0.,1.,0.));
#9934=DIRECTION('',(0.,0.,1.));
#9935=DIRECTION('center_axis',(0.,0.,1.));
#9936=DIRECTION('ref_axis',(1.,0.,0.));
#9937=DIRECTION('',(-1.,0.,0.));
#9938=DIRECTION('center_axis',(0.,1.,0.));
#9939=DIRECTION('ref_axis',(-1.,0.,0.));
#9940=DIRECTION('',(-1.,0.,0.));
#9941=DIRECTION('',(0.,0.,1.));
#9942=DIRECTION('',(1.,0.,0.));
#9943=DIRECTION('',(0.,0.,1.));
#9944=DIRECTION('center_axis',(1.,0.,0.));
#9945=DIRECTION('ref_axis',(0.,1.,0.));
#9946=DIRECTION('',(0.,1.,0.));
#9947=DIRECTION('',(0.,0.,-1.));
#9948=DIRECTION('',(0.,-1.,0.));
#9949=DIRECTION('center_axis',(-1.,0.,0.));
#9950=DIRECTION('ref_axis',(0.,-1.,0.));
#9951=DIRECTION('',(0.,-1.,0.));
#9952=DIRECTION('',(0.,1.,0.));
#9953=DIRECTION('',(0.,0.,1.));
#9954=DIRECTION('center_axis',(0.,0.,1.));
#9955=DIRECTION('ref_axis',(1.,0.,0.));
#9956=DIRECTION('',(-1.,0.,0.));
#9957=DIRECTION('center_axis',(0.,1.,0.));
#9958=DIRECTION('ref_axis',(-1.,0.,0.));
#9959=DIRECTION('',(-1.,0.,0.));
#9960=DIRECTION('',(0.,0.,1.));
#9961=DIRECTION('',(1.,0.,0.));
#9962=DIRECTION('',(0.,0.,1.));
#9963=DIRECTION('center_axis',(1.,0.,0.));
#9964=DIRECTION('ref_axis',(0.,1.,0.));
#9965=DIRECTION('',(0.,1.,0.));
#9966=DIRECTION('',(0.,0.,-1.));
#9967=DIRECTION('',(0.,-1.,0.));
#9968=DIRECTION('center_axis',(-1.,0.,0.));
#9969=DIRECTION('ref_axis',(0.,-1.,0.));
#9970=DIRECTION('',(0.,-1.,0.));
#9971=DIRECTION('',(0.,1.,0.));
#9972=DIRECTION('',(0.,0.,1.));
#9973=DIRECTION('center_axis',(0.,0.,1.));
#9974=DIRECTION('ref_axis',(1.,0.,0.));
#9975=DIRECTION('',(-1.,0.,0.));
#9976=DIRECTION('center_axis',(0.,1.,0.));
#9977=DIRECTION('ref_axis',(-1.,0.,0.));
#9978=DIRECTION('',(-1.,0.,0.));
#9979=DIRECTION('',(0.,0.,1.));
#9980=DIRECTION('',(1.,0.,0.));
#9981=DIRECTION('',(0.,0.,1.));
#9982=DIRECTION('center_axis',(1.,0.,0.));
#9983=DIRECTION('ref_axis',(0.,1.,0.));
#9984=DIRECTION('',(0.,1.,0.));
#9985=DIRECTION('',(0.,0.,-1.));
#9986=DIRECTION('',(0.,-1.,0.));
#9987=DIRECTION('center_axis',(-1.,0.,0.));
#9988=DIRECTION('ref_axis',(0.,-1.,0.));
#9989=DIRECTION('',(0.,-1.,0.));
#9990=DIRECTION('',(0.,1.,0.));
#9991=DIRECTION('',(0.,0.,1.));
#9992=DIRECTION('center_axis',(0.,0.,1.));
#9993=DIRECTION('ref_axis',(1.,0.,0.));
#9994=DIRECTION('',(-1.,0.,0.));
#9995=DIRECTION('center_axis',(0.,1.,0.));
#9996=DIRECTION('ref_axis',(-1.,0.,0.));
#9997=DIRECTION('',(-1.,0.,0.));
#9998=DIRECTION('',(0.,0.,1.));
#9999=DIRECTION('',(1.,0.,0.));
#10000=DIRECTION('',(0.,0.,1.));
#10001=DIRECTION('center_axis',(1.,0.,0.));
#10002=DIRECTION('ref_axis',(0.,1.,0.));
#10003=DIRECTION('',(0.,1.,0.));
#10004=DIRECTION('',(0.,0.,-1.));
#10005=DIRECTION('',(0.,-1.,0.));
#10006=DIRECTION('center_axis',(-1.,0.,0.));
#10007=DIRECTION('ref_axis',(0.,-1.,0.));
#10008=DIRECTION('',(0.,-1.,0.));
#10009=DIRECTION('',(0.,1.,0.));
#10010=DIRECTION('',(0.,0.,1.));
#10011=DIRECTION('center_axis',(0.,0.,1.));
#10012=DIRECTION('ref_axis',(1.,0.,0.));
#10013=DIRECTION('',(-1.,0.,0.));
#10014=DIRECTION('center_axis',(0.,1.,0.));
#10015=DIRECTION('ref_axis',(-1.,0.,0.));
#10016=DIRECTION('',(-1.,0.,0.));
#10017=DIRECTION('',(0.,0.,1.));
#10018=DIRECTION('',(1.,0.,0.));
#10019=DIRECTION('',(0.,0.,1.));
#10020=DIRECTION('center_axis',(1.,0.,0.));
#10021=DIRECTION('ref_axis',(0.,1.,0.));
#10022=DIRECTION('',(0.,1.,0.));
#10023=DIRECTION('',(0.,0.,-1.));
#10024=DIRECTION('',(0.,-1.,0.));
#10025=DIRECTION('center_axis',(-1.,0.,0.));
#10026=DIRECTION('ref_axis',(0.,-1.,0.));
#10027=DIRECTION('',(0.,-1.,0.));
#10028=DIRECTION('',(0.,1.,0.));
#10029=DIRECTION('',(0.,0.,1.));
#10030=DIRECTION('center_axis',(0.,0.,1.));
#10031=DIRECTION('ref_axis',(1.,0.,0.));
#10032=DIRECTION('',(-1.,0.,0.));
#10033=DIRECTION('center_axis',(0.,1.,0.));
#10034=DIRECTION('ref_axis',(-1.,0.,0.));
#10035=DIRECTION('',(-1.,0.,0.));
#10036=DIRECTION('',(0.,0.,1.));
#10037=DIRECTION('',(1.,0.,0.));
#10038=DIRECTION('',(0.,0.,1.));
#10039=DIRECTION('center_axis',(1.,0.,0.));
#10040=DIRECTION('ref_axis',(0.,1.,0.));
#10041=DIRECTION('',(0.,1.,0.));
#10042=DIRECTION('',(0.,0.,-1.));
#10043=DIRECTION('',(0.,-1.,0.));
#10044=DIRECTION('center_axis',(-1.,0.,0.));
#10045=DIRECTION('ref_axis',(0.,-1.,0.));
#10046=DIRECTION('',(0.,-1.,0.));
#10047=DIRECTION('',(0.,1.,0.));
#10048=DIRECTION('',(0.,0.,1.));
#10049=DIRECTION('center_axis',(0.,0.,1.));
#10050=DIRECTION('ref_axis',(1.,0.,0.));
#10051=DIRECTION('',(-1.,0.,0.));
#10052=DIRECTION('center_axis',(0.,1.,0.));
#10053=DIRECTION('ref_axis',(-1.,0.,0.));
#10054=DIRECTION('',(-1.,0.,0.));
#10055=DIRECTION('',(0.,0.,1.));
#10056=DIRECTION('',(1.,0.,0.));
#10057=DIRECTION('',(0.,0.,1.));
#10058=DIRECTION('center_axis',(1.,0.,0.));
#10059=DIRECTION('ref_axis',(0.,1.,0.));
#10060=DIRECTION('',(0.,1.,0.));
#10061=DIRECTION('',(0.,0.,-1.));
#10062=DIRECTION('',(0.,-1.,0.));
#10063=DIRECTION('center_axis',(-1.,0.,0.));
#10064=DIRECTION('ref_axis',(0.,-1.,0.));
#10065=DIRECTION('',(0.,-1.,0.));
#10066=DIRECTION('',(0.,1.,0.));
#10067=DIRECTION('',(0.,0.,1.));
#10068=DIRECTION('center_axis',(0.,0.,1.));
#10069=DIRECTION('ref_axis',(1.,0.,0.));
#10070=DIRECTION('',(-1.,0.,0.));
#10071=DIRECTION('center_axis',(0.,1.,0.));
#10072=DIRECTION('ref_axis',(-1.,0.,0.));
#10073=DIRECTION('',(-1.,0.,0.));
#10074=DIRECTION('',(0.,0.,1.));
#10075=DIRECTION('',(1.,0.,0.));
#10076=DIRECTION('',(0.,0.,1.));
#10077=DIRECTION('center_axis',(1.,0.,0.));
#10078=DIRECTION('ref_axis',(0.,1.,0.));
#10079=DIRECTION('',(0.,1.,0.));
#10080=DIRECTION('',(0.,0.,-1.));
#10081=DIRECTION('',(0.,-1.,0.));
#10082=DIRECTION('center_axis',(-1.,0.,0.));
#10083=DIRECTION('ref_axis',(0.,-1.,0.));
#10084=DIRECTION('',(0.,-1.,0.));
#10085=DIRECTION('',(0.,1.,0.));
#10086=DIRECTION('',(0.,0.,1.));
#10087=DIRECTION('center_axis',(0.,0.,1.));
#10088=DIRECTION('ref_axis',(1.,0.,0.));
#10089=DIRECTION('',(-1.,0.,0.));
#10090=DIRECTION('center_axis',(0.,1.,0.));
#10091=DIRECTION('ref_axis',(-1.,0.,0.));
#10092=DIRECTION('',(-1.,0.,0.));
#10093=DIRECTION('',(0.,0.,1.));
#10094=DIRECTION('',(1.,0.,0.));
#10095=DIRECTION('',(0.,0.,1.));
#10096=DIRECTION('center_axis',(1.,0.,0.));
#10097=DIRECTION('ref_axis',(0.,1.,0.));
#10098=DIRECTION('',(0.,1.,0.));
#10099=DIRECTION('',(0.,0.,-1.));
#10100=DIRECTION('',(0.,-1.,0.));
#10101=DIRECTION('center_axis',(-1.,0.,0.));
#10102=DIRECTION('ref_axis',(0.,-1.,0.));
#10103=DIRECTION('',(0.,-1.,0.));
#10104=DIRECTION('',(0.,1.,0.));
#10105=DIRECTION('',(0.,0.,1.));
#10106=DIRECTION('center_axis',(0.,0.,1.));
#10107=DIRECTION('ref_axis',(1.,0.,0.));
#10108=DIRECTION('',(-1.,0.,0.));
#10109=DIRECTION('center_axis',(0.,1.,0.));
#10110=DIRECTION('ref_axis',(-1.,0.,0.));
#10111=DIRECTION('',(-1.,0.,0.));
#10112=DIRECTION('',(0.,0.,1.));
#10113=DIRECTION('',(1.,0.,0.));
#10114=DIRECTION('',(0.,0.,1.));
#10115=DIRECTION('center_axis',(1.,0.,0.));
#10116=DIRECTION('ref_axis',(0.,1.,0.));
#10117=DIRECTION('',(0.,1.,0.));
#10118=DIRECTION('',(0.,0.,-1.));
#10119=DIRECTION('',(0.,-1.,0.));
#10120=DIRECTION('center_axis',(-1.,0.,0.));
#10121=DIRECTION('ref_axis',(0.,-1.,0.));
#10122=DIRECTION('',(0.,-1.,0.));
#10123=DIRECTION('',(0.,1.,0.));
#10124=DIRECTION('',(0.,0.,1.));
#10125=DIRECTION('center_axis',(0.,0.,1.));
#10126=DIRECTION('ref_axis',(1.,0.,0.));
#10127=DIRECTION('',(-1.,0.,0.));
#10128=DIRECTION('center_axis',(0.,1.,0.));
#10129=DIRECTION('ref_axis',(-1.,0.,0.));
#10130=DIRECTION('',(-1.,0.,0.));
#10131=DIRECTION('',(0.,0.,1.));
#10132=DIRECTION('',(1.,0.,0.));
#10133=DIRECTION('',(0.,0.,1.));
#10134=DIRECTION('center_axis',(1.,0.,0.));
#10135=DIRECTION('ref_axis',(0.,1.,0.));
#10136=DIRECTION('',(0.,1.,0.));
#10137=DIRECTION('',(0.,0.,-1.));
#10138=DIRECTION('',(0.,-1.,0.));
#10139=DIRECTION('center_axis',(-1.,0.,0.));
#10140=DIRECTION('ref_axis',(0.,-1.,0.));
#10141=DIRECTION('',(0.,-1.,0.));
#10142=DIRECTION('',(0.,1.,0.));
#10143=DIRECTION('',(0.,0.,1.));
#10144=DIRECTION('center_axis',(0.,0.,1.));
#10145=DIRECTION('ref_axis',(1.,0.,0.));
#10146=DIRECTION('',(-1.,0.,0.));
#10147=DIRECTION('center_axis',(0.,1.,0.));
#10148=DIRECTION('ref_axis',(-1.,0.,0.));
#10149=DIRECTION('',(-1.,0.,0.));
#10150=DIRECTION('',(0.,0.,1.));
#10151=DIRECTION('',(1.,0.,0.));
#10152=DIRECTION('',(0.,0.,1.));
#10153=DIRECTION('center_axis',(1.,0.,0.));
#10154=DIRECTION('ref_axis',(0.,1.,0.));
#10155=DIRECTION('',(0.,1.,0.));
#10156=DIRECTION('',(0.,0.,-1.));
#10157=DIRECTION('',(0.,-1.,0.));
#10158=DIRECTION('center_axis',(-1.,0.,0.));
#10159=DIRECTION('ref_axis',(0.,-1.,0.));
#10160=DIRECTION('',(0.,-1.,0.));
#10161=DIRECTION('',(0.,1.,0.));
#10162=DIRECTION('',(0.,0.,1.));
#10163=DIRECTION('center_axis',(0.,0.,1.));
#10164=DIRECTION('ref_axis',(1.,0.,0.));
#10165=DIRECTION('',(-1.,0.,0.));
#10166=DIRECTION('center_axis',(0.,1.,0.));
#10167=DIRECTION('ref_axis',(-1.,0.,0.));
#10168=DIRECTION('',(-1.,0.,0.));
#10169=DIRECTION('',(0.,0.,1.));
#10170=DIRECTION('',(1.,0.,0.));
#10171=DIRECTION('',(0.,0.,1.));
#10172=DIRECTION('center_axis',(1.,0.,0.));
#10173=DIRECTION('ref_axis',(0.,1.,0.));
#10174=DIRECTION('',(0.,1.,0.));
#10175=DIRECTION('',(0.,0.,-1.));
#10176=DIRECTION('',(0.,-1.,0.));
#10177=DIRECTION('center_axis',(-1.,0.,0.));
#10178=DIRECTION('ref_axis',(0.,-1.,0.));
#10179=DIRECTION('',(0.,-1.,0.));
#10180=DIRECTION('',(0.,1.,0.));
#10181=DIRECTION('',(0.,0.,1.));
#10182=DIRECTION('center_axis',(0.,0.,1.));
#10183=DIRECTION('ref_axis',(1.,0.,0.));
#10184=DIRECTION('',(-1.,0.,0.));
#10185=DIRECTION('center_axis',(0.,1.,0.));
#10186=DIRECTION('ref_axis',(-1.,0.,0.));
#10187=DIRECTION('',(-1.,0.,0.));
#10188=DIRECTION('',(0.,0.,1.));
#10189=DIRECTION('',(1.,0.,0.));
#10190=DIRECTION('',(0.,0.,1.));
#10191=DIRECTION('center_axis',(1.,0.,0.));
#10192=DIRECTION('ref_axis',(0.,1.,0.));
#10193=DIRECTION('',(0.,1.,0.));
#10194=DIRECTION('',(0.,0.,-1.));
#10195=DIRECTION('',(0.,-1.,0.));
#10196=DIRECTION('center_axis',(-1.,0.,0.));
#10197=DIRECTION('ref_axis',(0.,-1.,0.));
#10198=DIRECTION('',(0.,-1.,0.));
#10199=DIRECTION('',(0.,1.,0.));
#10200=DIRECTION('',(0.,0.,1.));
#10201=DIRECTION('center_axis',(0.,0.,1.));
#10202=DIRECTION('ref_axis',(1.,0.,0.));
#10203=DIRECTION('',(-1.,0.,0.));
#10204=DIRECTION('center_axis',(0.,1.,0.));
#10205=DIRECTION('ref_axis',(-1.,0.,0.));
#10206=DIRECTION('',(-1.,0.,0.));
#10207=DIRECTION('',(0.,0.,1.));
#10208=DIRECTION('',(1.,0.,0.));
#10209=DIRECTION('',(0.,0.,1.));
#10210=DIRECTION('center_axis',(1.,0.,0.));
#10211=DIRECTION('ref_axis',(0.,1.,0.));
#10212=DIRECTION('',(0.,1.,0.));
#10213=DIRECTION('',(0.,0.,-1.));
#10214=DIRECTION('',(0.,-1.,0.));
#10215=DIRECTION('center_axis',(-1.,0.,0.));
#10216=DIRECTION('ref_axis',(0.,-1.,0.));
#10217=DIRECTION('',(0.,-1.,0.));
#10218=DIRECTION('',(0.,1.,0.));
#10219=DIRECTION('',(0.,0.,1.));
#10220=DIRECTION('center_axis',(0.,0.,1.));
#10221=DIRECTION('ref_axis',(1.,0.,0.));
#10222=DIRECTION('',(-1.,0.,0.));
#10223=DIRECTION('center_axis',(0.,1.,0.));
#10224=DIRECTION('ref_axis',(-1.,0.,0.));
#10225=DIRECTION('',(-1.,0.,0.));
#10226=DIRECTION('',(0.,0.,1.));
#10227=DIRECTION('',(1.,0.,0.));
#10228=DIRECTION('',(0.,0.,1.));
#10229=DIRECTION('center_axis',(1.,0.,0.));
#10230=DIRECTION('ref_axis',(0.,1.,0.));
#10231=DIRECTION('',(0.,1.,0.));
#10232=DIRECTION('',(0.,0.,-1.));
#10233=DIRECTION('',(0.,-1.,0.));
#10234=DIRECTION('center_axis',(-1.,0.,0.));
#10235=DIRECTION('ref_axis',(0.,-1.,0.));
#10236=DIRECTION('',(0.,-1.,0.));
#10237=DIRECTION('',(0.,1.,0.));
#10238=DIRECTION('',(0.,0.,1.));
#10239=DIRECTION('center_axis',(0.,0.,1.));
#10240=DIRECTION('ref_axis',(1.,0.,0.));
#10241=DIRECTION('',(-1.,0.,0.));
#10242=DIRECTION('center_axis',(0.,1.,0.));
#10243=DIRECTION('ref_axis',(-1.,0.,0.));
#10244=DIRECTION('',(-1.,0.,0.));
#10245=DIRECTION('',(0.,0.,1.));
#10246=DIRECTION('',(1.,0.,0.));
#10247=DIRECTION('',(0.,0.,1.));
#10248=DIRECTION('center_axis',(1.,0.,0.));
#10249=DIRECTION('ref_axis',(0.,1.,0.));
#10250=DIRECTION('',(0.,1.,0.));
#10251=DIRECTION('',(0.,0.,-1.));
#10252=DIRECTION('',(0.,-1.,0.));
#10253=DIRECTION('center_axis',(-1.,0.,0.));
#10254=DIRECTION('ref_axis',(0.,-1.,0.));
#10255=DIRECTION('',(0.,-1.,0.));
#10256=DIRECTION('',(0.,1.,0.));
#10257=DIRECTION('',(0.,0.,1.));
#10258=DIRECTION('center_axis',(0.,0.,1.));
#10259=DIRECTION('ref_axis',(1.,0.,0.));
#10260=DIRECTION('',(-1.,0.,0.));
#10261=DIRECTION('center_axis',(0.,1.,0.));
#10262=DIRECTION('ref_axis',(-1.,0.,0.));
#10263=DIRECTION('',(-1.,0.,0.));
#10264=DIRECTION('',(0.,0.,1.));
#10265=DIRECTION('',(1.,0.,0.));
#10266=DIRECTION('',(0.,0.,1.));
#10267=DIRECTION('center_axis',(1.,0.,0.));
#10268=DIRECTION('ref_axis',(0.,1.,0.));
#10269=DIRECTION('',(0.,1.,0.));
#10270=DIRECTION('',(0.,0.,-1.));
#10271=DIRECTION('',(0.,-1.,0.));
#10272=DIRECTION('center_axis',(-1.,0.,0.));
#10273=DIRECTION('ref_axis',(0.,-1.,0.));
#10274=DIRECTION('',(0.,-1.,0.));
#10275=DIRECTION('',(0.,1.,0.));
#10276=DIRECTION('',(0.,0.,1.));
#10277=DIRECTION('center_axis',(0.,0.,1.));
#10278=DIRECTION('ref_axis',(1.,0.,0.));
#10279=DIRECTION('',(-1.,0.,0.));
#10280=DIRECTION('center_axis',(0.,1.,0.));
#10281=DIRECTION('ref_axis',(-1.,0.,0.));
#10282=DIRECTION('',(-1.,0.,0.));
#10283=DIRECTION('',(0.,0.,1.));
#10284=DIRECTION('',(1.,0.,0.));
#10285=DIRECTION('',(0.,0.,1.));
#10286=DIRECTION('center_axis',(1.,0.,0.));
#10287=DIRECTION('ref_axis',(0.,1.,0.));
#10288=DIRECTION('',(0.,1.,0.));
#10289=DIRECTION('',(0.,0.,-1.));
#10290=DIRECTION('',(0.,-1.,0.));
#10291=DIRECTION('center_axis',(-1.,0.,0.));
#10292=DIRECTION('ref_axis',(0.,-1.,0.));
#10293=DIRECTION('',(0.,-1.,0.));
#10294=DIRECTION('',(0.,1.,0.));
#10295=DIRECTION('',(0.,0.,1.));
#10296=DIRECTION('center_axis',(0.,0.,1.));
#10297=DIRECTION('ref_axis',(1.,0.,0.));
#10298=DIRECTION('',(-1.,0.,0.));
#10299=DIRECTION('center_axis',(0.,1.,0.));
#10300=DIRECTION('ref_axis',(-1.,0.,0.));
#10301=DIRECTION('',(-1.,0.,0.));
#10302=DIRECTION('',(0.,0.,1.));
#10303=DIRECTION('',(1.,0.,0.));
#10304=DIRECTION('',(0.,0.,1.));
#10305=DIRECTION('center_axis',(1.,0.,0.));
#10306=DIRECTION('ref_axis',(0.,1.,0.));
#10307=DIRECTION('',(0.,1.,0.));
#10308=DIRECTION('',(0.,0.,-1.));
#10309=DIRECTION('',(0.,-1.,0.));
#10310=DIRECTION('center_axis',(-1.,0.,0.));
#10311=DIRECTION('ref_axis',(0.,-1.,0.));
#10312=DIRECTION('',(0.,-1.,0.));
#10313=DIRECTION('',(0.,1.,0.));
#10314=DIRECTION('',(0.,0.,1.));
#10315=DIRECTION('center_axis',(0.,0.,1.));
#10316=DIRECTION('ref_axis',(1.,0.,0.));
#10317=DIRECTION('',(-1.,0.,0.));
#10318=DIRECTION('center_axis',(0.,1.,0.));
#10319=DIRECTION('ref_axis',(-1.,0.,0.));
#10320=DIRECTION('',(-1.,0.,0.));
#10321=DIRECTION('',(0.,0.,1.));
#10322=DIRECTION('',(1.,0.,0.));
#10323=DIRECTION('',(0.,0.,1.));
#10324=DIRECTION('center_axis',(1.,0.,0.));
#10325=DIRECTION('ref_axis',(0.,1.,0.));
#10326=DIRECTION('',(0.,1.,0.));
#10327=DIRECTION('',(0.,0.,-1.));
#10328=DIRECTION('',(0.,-1.,0.));
#10329=DIRECTION('center_axis',(-1.,0.,0.));
#10330=DIRECTION('ref_axis',(0.,-1.,0.));
#10331=DIRECTION('',(0.,-1.,0.));
#10332=DIRECTION('',(0.,1.,0.));
#10333=DIRECTION('',(0.,0.,1.));
#10334=DIRECTION('center_axis',(0.,0.,1.));
#10335=DIRECTION('ref_axis',(1.,0.,0.));
#10336=DIRECTION('',(-1.,0.,0.));
#10337=DIRECTION('center_axis',(0.,1.,0.));
#10338=DIRECTION('ref_axis',(-1.,0.,0.));
#10339=DIRECTION('',(-1.,0.,0.));
#10340=DIRECTION('',(0.,0.,1.));
#10341=DIRECTION('',(1.,0.,0.));
#10342=DIRECTION('',(0.,0.,1.));
#10343=DIRECTION('center_axis',(1.,0.,0.));
#10344=DIRECTION('ref_axis',(0.,1.,0.));
#10345=DIRECTION('',(0.,1.,0.));
#10346=DIRECTION('',(0.,0.,-1.));
#10347=DIRECTION('',(0.,-1.,0.));
#10348=DIRECTION('center_axis',(-1.,0.,0.));
#10349=DIRECTION('ref_axis',(0.,-1.,0.));
#10350=DIRECTION('',(0.,-1.,0.));
#10351=DIRECTION('',(0.,1.,0.));
#10352=DIRECTION('',(0.,0.,1.));
#10353=DIRECTION('center_axis',(0.,0.,1.));
#10354=DIRECTION('ref_axis',(1.,0.,0.));
#10355=DIRECTION('',(-1.,0.,0.));
#10356=DIRECTION('center_axis',(0.,1.,0.));
#10357=DIRECTION('ref_axis',(-1.,0.,0.));
#10358=DIRECTION('',(-1.,0.,0.));
#10359=DIRECTION('',(0.,0.,1.));
#10360=DIRECTION('',(1.,0.,0.));
#10361=DIRECTION('',(0.,0.,1.));
#10362=DIRECTION('center_axis',(1.,0.,0.));
#10363=DIRECTION('ref_axis',(0.,1.,0.));
#10364=DIRECTION('',(0.,1.,0.));
#10365=DIRECTION('',(0.,0.,-1.));
#10366=DIRECTION('',(0.,-1.,0.));
#10367=DIRECTION('center_axis',(-1.,0.,0.));
#10368=DIRECTION('ref_axis',(0.,-1.,0.));
#10369=DIRECTION('',(0.,-1.,0.));
#10370=DIRECTION('',(0.,1.,0.));
#10371=DIRECTION('',(0.,0.,1.));
#10372=DIRECTION('center_axis',(0.,0.,1.));
#10373=DIRECTION('ref_axis',(1.,0.,0.));
#10374=DIRECTION('',(-1.,0.,0.));
#10375=DIRECTION('center_axis',(0.,1.,0.));
#10376=DIRECTION('ref_axis',(-1.,0.,0.));
#10377=DIRECTION('',(-1.,0.,0.));
#10378=DIRECTION('',(0.,0.,1.));
#10379=DIRECTION('',(1.,0.,0.));
#10380=DIRECTION('',(0.,0.,1.));
#10381=DIRECTION('center_axis',(1.,0.,0.));
#10382=DIRECTION('ref_axis',(0.,1.,0.));
#10383=DIRECTION('',(0.,1.,0.));
#10384=DIRECTION('',(0.,0.,-1.));
#10385=DIRECTION('',(0.,-1.,0.));
#10386=DIRECTION('center_axis',(-1.,0.,0.));
#10387=DIRECTION('ref_axis',(0.,-1.,0.));
#10388=DIRECTION('',(0.,-1.,0.));
#10389=DIRECTION('',(0.,1.,0.));
#10390=DIRECTION('',(0.,0.,1.));
#10391=DIRECTION('center_axis',(0.,0.,1.));
#10392=DIRECTION('ref_axis',(1.,0.,0.));
#10393=DIRECTION('',(-1.,0.,0.));
#10394=DIRECTION('center_axis',(0.,1.,0.));
#10395=DIRECTION('ref_axis',(-1.,0.,0.));
#10396=DIRECTION('',(-1.,0.,0.));
#10397=DIRECTION('',(0.,0.,1.));
#10398=DIRECTION('',(1.,0.,0.));
#10399=DIRECTION('',(0.,0.,1.));
#10400=DIRECTION('center_axis',(1.,0.,0.));
#10401=DIRECTION('ref_axis',(0.,1.,0.));
#10402=DIRECTION('',(0.,1.,0.));
#10403=DIRECTION('',(0.,0.,-1.));
#10404=DIRECTION('',(0.,-1.,0.));
#10405=DIRECTION('center_axis',(-1.,0.,0.));
#10406=DIRECTION('ref_axis',(0.,-1.,0.));
#10407=DIRECTION('',(0.,-1.,0.));
#10408=DIRECTION('',(0.,1.,0.));
#10409=DIRECTION('',(0.,0.,1.));
#10410=DIRECTION('center_axis',(0.,0.,1.));
#10411=DIRECTION('ref_axis',(1.,0.,0.));
#10412=DIRECTION('',(-1.,0.,0.));
#10413=DIRECTION('center_axis',(0.,1.,0.));
#10414=DIRECTION('ref_axis',(-1.,0.,0.));
#10415=DIRECTION('',(-1.,0.,0.));
#10416=DIRECTION('',(0.,0.,1.));
#10417=DIRECTION('',(1.,0.,0.));
#10418=DIRECTION('',(0.,0.,1.));
#10419=DIRECTION('center_axis',(1.,0.,0.));
#10420=DIRECTION('ref_axis',(0.,1.,0.));
#10421=DIRECTION('',(0.,1.,0.));
#10422=DIRECTION('',(0.,0.,-1.));
#10423=DIRECTION('',(0.,-1.,0.));
#10424=DIRECTION('center_axis',(-1.,0.,0.));
#10425=DIRECTION('ref_axis',(0.,-1.,0.));
#10426=DIRECTION('',(0.,-1.,0.));
#10427=DIRECTION('',(0.,1.,0.));
#10428=DIRECTION('',(0.,0.,1.));
#10429=DIRECTION('center_axis',(0.,0.,1.));
#10430=DIRECTION('ref_axis',(1.,0.,0.));
#10431=DIRECTION('',(-1.,0.,0.));
#10432=DIRECTION('center_axis',(0.,1.,0.));
#10433=DIRECTION('ref_axis',(-1.,0.,0.));
#10434=DIRECTION('',(-1.,0.,0.));
#10435=DIRECTION('',(0.,0.,1.));
#10436=DIRECTION('',(1.,0.,0.));
#10437=DIRECTION('',(0.,0.,1.));
#10438=DIRECTION('center_axis',(1.,0.,0.));
#10439=DIRECTION('ref_axis',(0.,1.,0.));
#10440=DIRECTION('',(0.,1.,0.));
#10441=DIRECTION('',(0.,0.,-1.));
#10442=DIRECTION('',(0.,-1.,0.));
#10443=DIRECTION('center_axis',(-1.,0.,0.));
#10444=DIRECTION('ref_axis',(0.,-1.,0.));
#10445=DIRECTION('',(0.,-1.,0.));
#10446=DIRECTION('',(0.,1.,0.));
#10447=DIRECTION('',(0.,0.,1.));
#10448=DIRECTION('center_axis',(0.,0.,1.));
#10449=DIRECTION('ref_axis',(1.,0.,0.));
#10450=DIRECTION('',(-1.,0.,0.));
#10451=DIRECTION('center_axis',(0.,1.,0.));
#10452=DIRECTION('ref_axis',(-1.,0.,0.));
#10453=DIRECTION('',(-1.,0.,0.));
#10454=DIRECTION('',(0.,0.,1.));
#10455=DIRECTION('',(1.,0.,0.));
#10456=DIRECTION('',(0.,0.,1.));
#10457=DIRECTION('center_axis',(1.,0.,0.));
#10458=DIRECTION('ref_axis',(0.,1.,0.));
#10459=DIRECTION('',(0.,1.,0.));
#10460=DIRECTION('',(0.,0.,-1.));
#10461=DIRECTION('',(0.,-1.,0.));
#10462=DIRECTION('center_axis',(-1.,0.,0.));
#10463=DIRECTION('ref_axis',(0.,-1.,0.));
#10464=DIRECTION('',(0.,-1.,0.));
#10465=DIRECTION('',(0.,1.,0.));
#10466=DIRECTION('',(0.,0.,1.));
#10467=DIRECTION('center_axis',(0.,0.,1.));
#10468=DIRECTION('ref_axis',(1.,0.,0.));
#10469=DIRECTION('',(-1.,0.,0.));
#10470=DIRECTION('center_axis',(0.,0.,1.));
#10471=DIRECTION('ref_axis',(1.,0.,0.));
#10472=DIRECTION('',(1.,0.,0.));
#10473=DIRECTION('',(1.,0.,0.));
#10474=DIRECTION('',(0.,1.,0.));
#10475=DIRECTION('',(-1.,0.,0.));
#10476=DIRECTION('',(0.,-1.,0.));
#10477=DIRECTION('',(1.,0.,0.));
#10478=DIRECTION('',(1.,0.,0.));
#10479=DIRECTION('',(1.,0.,0.));
#10480=DIRECTION('',(1.,0.,0.));
#10481=DIRECTION('',(1.,0.,0.));
#10482=DIRECTION('',(1.,0.,0.));
#10483=DIRECTION('',(1.,0.,0.));
#10484=DIRECTION('',(1.,0.,0.));
#10485=DIRECTION('',(1.,0.,0.));
#10486=DIRECTION('',(1.,0.,0.));
#10487=DIRECTION('',(1.,0.,0.));
#10488=DIRECTION('',(1.,0.,0.));
#10489=DIRECTION('',(1.,0.,0.));
#10490=DIRECTION('',(1.,0.,0.));
#10491=DIRECTION('',(1.,0.,0.));
#10492=DIRECTION('',(1.,0.,0.));
#10493=DIRECTION('',(1.,0.,0.));
#10494=DIRECTION('',(1.,0.,0.));
#10495=DIRECTION('',(1.,0.,0.));
#10496=DIRECTION('',(1.,0.,0.));
#10497=DIRECTION('',(1.,0.,0.));
#10498=DIRECTION('',(1.,0.,0.));
#10499=DIRECTION('',(1.,0.,0.));
#10500=DIRECTION('',(1.,0.,0.));
#10501=DIRECTION('',(1.,0.,0.));
#10502=DIRECTION('',(1.,0.,0.));
#10503=DIRECTION('',(1.,0.,0.));
#10504=DIRECTION('',(1.,0.,0.));
#10505=DIRECTION('center_axis',(0.,0.,-1.));
#10506=DIRECTION('ref_axis',(1.,0.,0.));
#10507=DIRECTION('center_axis',(0.,0.,-1.));
#10508=DIRECTION('ref_axis',(1.,0.,0.));
#10509=DIRECTION('center_axis',(0.,0.,1.));
#10510=DIRECTION('ref_axis',(1.,0.,0.));
#10511=DIRECTION('center_axis',(0.,0.,1.));
#10512=DIRECTION('ref_axis',(1.,0.,0.));
#10513=DIRECTION('',(0.,0.,1.));
#10514=DIRECTION('center_axis',(0.,0.,1.));
#10515=DIRECTION('ref_axis',(1.,0.,0.));
#10516=DIRECTION('center_axis',(0.,0.,1.));
#10517=DIRECTION('ref_axis',(1.,0.,0.));
#10518=DIRECTION('',(0.,0.,1.));
#10519=DIRECTION('center_axis',(0.,1.,0.));
#10520=DIRECTION('ref_axis',(-1.,0.,0.));
#10521=DIRECTION('',(-1.,0.,0.));
#10522=DIRECTION('',(0.,0.,1.));
#10523=DIRECTION('',(0.,0.,1.));
#10524=DIRECTION('center_axis',(1.,0.,0.));
#10525=DIRECTION('ref_axis',(0.,1.,0.));
#10526=DIRECTION('',(0.,1.,0.));
#10527=DIRECTION('',(0.,0.,1.));
#10528=DIRECTION('center_axis',(0.,-1.,0.));
#10529=DIRECTION('ref_axis',(1.,0.,0.));
#10530=DIRECTION('',(0.,0.,1.));
#10531=DIRECTION('',(1.,0.,0.));
#10532=DIRECTION('center_axis',(-1.,0.,0.));
#10533=DIRECTION('ref_axis',(0.,-1.,0.));
#10534=DIRECTION('',(0.,-1.,0.));
#10535=DIRECTION('center_axis',(0.,0.,1.));
#10536=DIRECTION('ref_axis',(1.,0.,0.));
#10537=DIRECTION('axis',(0.,0.,1.));
#10538=DIRECTION('refdir',(1.,0.,0.));
#10539=DIRECTION('center_axis',(0.,1.,0.));
#10540=DIRECTION('ref_axis',(-1.,0.,0.));
#10541=DIRECTION('',(-1.,0.,0.));
#10542=DIRECTION('',(0.,0.,1.));
#10543=DIRECTION('',(-1.,0.,0.));
#10544=DIRECTION('',(0.,0.,1.));
#10545=DIRECTION('center_axis',(1.,0.,0.));
#10546=DIRECTION('ref_axis',(0.,1.,0.));
#10547=DIRECTION('',(0.,1.,0.));
#10548=DIRECTION('',(0.,1.,0.));
#10549=DIRECTION('',(0.,0.,1.));
#10550=DIRECTION('center_axis',(0.,-1.,0.));
#10551=DIRECTION('ref_axis',(1.,0.,0.));
#10552=DIRECTION('',(1.,0.,0.));
#10553=DIRECTION('',(1.,0.,0.));
#10554=DIRECTION('',(0.,0.,1.));
#10555=DIRECTION('center_axis',(-1.,0.,0.));
#10556=DIRECTION('ref_axis',(0.,-1.,0.));
#10557=DIRECTION('',(0.,-1.,0.));
#10558=DIRECTION('',(0.,-1.,0.));
#10559=DIRECTION('center_axis',(0.,0.,1.));
#10560=DIRECTION('ref_axis',(1.,0.,0.));
#10561=DIRECTION('center_axis',(0.,0.,1.));
#10562=DIRECTION('ref_axis',(1.,0.,0.));
#10563=DIRECTION('axis',(0.,0.,1.));
#10564=DIRECTION('refdir',(1.,0.,0.));
#10565=DIRECTION('center_axis',(0.,1.,0.));
#10566=DIRECTION('ref_axis',(-1.,0.,0.));
#10567=DIRECTION('',(-1.,0.,0.));
#10568=DIRECTION('',(0.,0.,1.));
#10569=DIRECTION('',(-1.,0.,0.));
#10570=DIRECTION('',(0.,0.,1.));
#10571=DIRECTION('center_axis',(1.,0.,0.));
#10572=DIRECTION('ref_axis',(0.,1.,0.));
#10573=DIRECTION('',(0.,1.,0.));
#10574=DIRECTION('',(0.,1.,0.));
#10575=DIRECTION('',(0.,0.,1.));
#10576=DIRECTION('center_axis',(0.,-1.,0.));
#10577=DIRECTION('ref_axis',(1.,0.,0.));
#10578=DIRECTION('',(1.,0.,0.));
#10579=DIRECTION('',(1.,0.,0.));
#10580=DIRECTION('',(0.,0.,1.));
#10581=DIRECTION('center_axis',(-1.,0.,0.));
#10582=DIRECTION('ref_axis',(0.,-1.,0.));
#10583=DIRECTION('',(0.,-1.,0.));
#10584=DIRECTION('',(0.,-1.,0.));
#10585=DIRECTION('center_axis',(0.,0.,1.));
#10586=DIRECTION('ref_axis',(1.,0.,0.));
#10587=DIRECTION('center_axis',(0.,0.,1.));
#10588=DIRECTION('ref_axis',(1.,0.,0.));
#10589=DIRECTION('axis',(0.,0.,1.));
#10590=DIRECTION('refdir',(1.,0.,0.));
#10591=DIRECTION('center_axis',(0.,1.,0.));
#10592=DIRECTION('ref_axis',(-1.,0.,0.));
#10593=DIRECTION('',(-1.,0.,0.));
#10594=DIRECTION('',(0.,0.,1.));
#10595=DIRECTION('',(-1.,0.,0.));
#10596=DIRECTION('',(0.,0.,1.));
#10597=DIRECTION('center_axis',(1.,0.,0.));
#10598=DIRECTION('ref_axis',(0.,1.,0.));
#10599=DIRECTION('',(0.,1.,0.));
#10600=DIRECTION('',(0.,1.,0.));
#10601=DIRECTION('',(0.,0.,1.));
#10602=DIRECTION('center_axis',(0.,-1.,0.));
#10603=DIRECTION('ref_axis',(1.,0.,0.));
#10604=DIRECTION('',(1.,0.,0.));
#10605=DIRECTION('',(1.,0.,0.));
#10606=DIRECTION('',(0.,0.,1.));
#10607=DIRECTION('center_axis',(-1.,0.,0.));
#10608=DIRECTION('ref_axis',(0.,-1.,0.));
#10609=DIRECTION('',(0.,-1.,0.));
#10610=DIRECTION('',(0.,-1.,0.));
#10611=DIRECTION('center_axis',(0.,0.,1.));
#10612=DIRECTION('ref_axis',(1.,0.,0.));
#10613=DIRECTION('center_axis',(0.,0.,1.));
#10614=DIRECTION('ref_axis',(1.,0.,0.));
#10615=DIRECTION('axis',(0.,0.,1.));
#10616=DIRECTION('refdir',(1.,0.,0.));
#10617=DIRECTION('center_axis',(0.,1.,0.));
#10618=DIRECTION('ref_axis',(-1.,0.,0.));
#10619=DIRECTION('',(-1.,0.,0.));
#10620=DIRECTION('',(0.,0.,1.));
#10621=DIRECTION('',(-1.,0.,0.));
#10622=DIRECTION('',(0.,0.,1.));
#10623=DIRECTION('center_axis',(1.,0.,0.));
#10624=DIRECTION('ref_axis',(0.,1.,0.));
#10625=DIRECTION('',(0.,1.,0.));
#10626=DIRECTION('',(0.,1.,0.));
#10627=DIRECTION('',(0.,0.,1.));
#10628=DIRECTION('center_axis',(0.,-1.,0.));
#10629=DIRECTION('ref_axis',(1.,0.,0.));
#10630=DIRECTION('',(1.,0.,0.));
#10631=DIRECTION('',(1.,0.,0.));
#10632=DIRECTION('',(0.,0.,1.));
#10633=DIRECTION('center_axis',(-1.,0.,0.));
#10634=DIRECTION('ref_axis',(0.,-1.,0.));
#10635=DIRECTION('',(0.,-1.,0.));
#10636=DIRECTION('',(0.,-1.,0.));
#10637=DIRECTION('center_axis',(0.,0.,1.));
#10638=DIRECTION('ref_axis',(1.,0.,0.));
#10639=DIRECTION('center_axis',(0.,0.,1.));
#10640=DIRECTION('ref_axis',(1.,0.,0.));
#10641=DIRECTION('axis',(0.,0.,1.));
#10642=DIRECTION('refdir',(1.,0.,0.));
#10643=DIRECTION('center_axis',(0.,0.,1.));
#10644=DIRECTION('ref_axis',(1.,0.,0.));
#10645=DIRECTION('center_axis',(0.,0.,1.));
#10646=DIRECTION('ref_axis',(1.,0.,0.));
#10647=DIRECTION('',(0.,0.,1.));
#10648=DIRECTION('center_axis',(0.,0.,-1.));
#10649=DIRECTION('ref_axis',(1.,0.,0.));
#10650=DIRECTION('center_axis',(0.,0.,1.));
#10651=DIRECTION('ref_axis',(1.,0.,0.));
#10652=DIRECTION('center_axis',(0.,0.,1.));
#10653=DIRECTION('ref_axis',(1.,0.,0.));
#10654=DIRECTION('center_axis',(0.,0.,1.));
#10655=DIRECTION('ref_axis',(1.,0.,0.));
#10656=DIRECTION('center_axis',(0.,0.,1.));
#10657=DIRECTION('ref_axis',(1.,0.,0.));
#10658=DIRECTION('',(0.,0.,1.));
#10659=DIRECTION('center_axis',(0.,0.,-1.));
#10660=DIRECTION('ref_axis',(1.,0.,0.));
#10661=DIRECTION('center_axis',(0.,0.,1.));
#10662=DIRECTION('ref_axis',(1.,0.,0.));
#10663=DIRECTION('center_axis',(0.,0.,1.));
#10664=DIRECTION('ref_axis',(1.,0.,0.));
#10665=DIRECTION('center_axis',(0.,0.,1.));
#10666=DIRECTION('ref_axis',(1.,0.,0.));
#10667=DIRECTION('center_axis',(0.,0.,1.));
#10668=DIRECTION('ref_axis',(1.,0.,0.));
#10669=DIRECTION('',(0.,0.,1.));
#10670=DIRECTION('center_axis',(0.,0.,-1.));
#10671=DIRECTION('ref_axis',(1.,0.,0.));
#10672=DIRECTION('center_axis',(0.,0.,1.));
#10673=DIRECTION('ref_axis',(1.,0.,0.));
#10674=DIRECTION('center_axis',(0.,0.,1.));
#10675=DIRECTION('ref_axis',(1.,0.,0.));
#10676=DIRECTION('center_axis',(0.,0.,1.));
#10677=DIRECTION('ref_axis',(1.,0.,0.));
#10678=DIRECTION('center_axis',(0.,0.,1.));
#10679=DIRECTION('ref_axis',(1.,0.,0.));
#10680=DIRECTION('',(0.,0.,1.));
#10681=DIRECTION('center_axis',(0.,0.,-1.));
#10682=DIRECTION('ref_axis',(1.,0.,0.));
#10683=DIRECTION('center_axis',(0.,0.,1.));
#10684=DIRECTION('ref_axis',(1.,0.,0.));
#10685=DIRECTION('center_axis',(0.,0.,1.));
#10686=DIRECTION('ref_axis',(1.,0.,0.));
#10687=DIRECTION('center_axis',(0.,0.,1.));
#10688=DIRECTION('ref_axis',(1.,0.,0.));
#10689=DIRECTION('center_axis',(0.,0.,1.));
#10690=DIRECTION('ref_axis',(1.,0.,0.));
#10691=DIRECTION('',(0.,0.,1.));
#10692=DIRECTION('center_axis',(0.,0.,1.));
#10693=DIRECTION('ref_axis',(1.,0.,0.));
#10694=DIRECTION('center_axis',(0.,0.,1.));
#10695=DIRECTION('ref_axis',(1.,0.,0.));
#10696=DIRECTION('',(0.,0.,1.));
#10697=DIRECTION('center_axis',(0.,0.,1.));
#10698=DIRECTION('ref_axis',(1.,0.,0.));
#10699=DIRECTION('center_axis',(0.,0.,1.));
#10700=DIRECTION('ref_axis',(1.,0.,0.));
#10701=DIRECTION('',(0.,0.,1.));
#10702=DIRECTION('center_axis',(0.,0.,1.));
#10703=DIRECTION('ref_axis',(1.,0.,0.));
#10704=DIRECTION('center_axis',(0.,0.,1.));
#10705=DIRECTION('ref_axis',(1.,0.,0.));
#10706=DIRECTION('',(0.,0.,1.));
#10707=DIRECTION('center_axis',(0.,-0.56333682464151,0.826227342807548));
#10708=DIRECTION('ref_axis',(0.,-0.826227342807548,-0.56333682464151));
#10709=DIRECTION('',(0.,-0.826227342807548,-0.56333682464151));
#10710=DIRECTION('',(1.,0.,0.));
#10711=DIRECTION('',(0.,-0.826227342807548,-0.56333682464151));
#10712=DIRECTION('',(1.,0.,0.));
#10713=DIRECTION('center_axis',(0.,-1.,0.));
#10714=DIRECTION('ref_axis',(0.,0.,-1.));
#10715=DIRECTION('',(0.,0.,-1.));
#10716=DIRECTION('',(0.,0.,-1.));
#10717=DIRECTION('',(1.,0.,0.));
#10718=DIRECTION('center_axis',(0.,-0.56333682464151,-0.826227342807548));
#10719=DIRECTION('ref_axis',(0.,0.826227342807548,-0.56333682464151));
#10720=DIRECTION('',(0.,0.826227342807548,-0.56333682464151));
#10721=DIRECTION('',(0.,0.826227342807548,-0.56333682464151));
#10722=DIRECTION('',(1.,0.,0.));
#10723=DIRECTION('center_axis',(0.,-1.,0.));
#10724=DIRECTION('ref_axis',(0.,0.,-1.));
#10725=DIRECTION('',(0.,0.,-1.));
#10726=DIRECTION('',(0.,0.,-1.));
#10727=DIRECTION('',(1.,0.,0.));
#10728=DIRECTION('center_axis',(0.,0.,1.));
#10729=DIRECTION('ref_axis',(0.,-1.,0.));
#10730=DIRECTION('',(0.,-1.,0.));
#10731=DIRECTION('',(0.,-1.,0.));
#10732=DIRECTION('',(1.,0.,0.));
#10733=DIRECTION('center_axis',(0.,1.,0.));
#10734=DIRECTION('ref_axis',(0.,0.,1.));
#10735=DIRECTION('',(0.,0.,1.));
#10736=DIRECTION('',(0.,0.,1.));
#10737=DIRECTION('',(1.,0.,0.));
#10738=DIRECTION('center_axis',(0.,0.56333682464151,-0.826227342807548));
#10739=DIRECTION('ref_axis',(0.,0.826227342807548,0.56333682464151));
#10740=DIRECTION('',(0.,0.826227342807548,0.56333682464151));
#10741=DIRECTION('',(0.,0.826227342807548,0.56333682464151));
#10742=DIRECTION('',(1.,0.,0.));
#10743=DIRECTION('center_axis',(0.,1.,0.));
#10744=DIRECTION('ref_axis',(0.,0.,1.));
#10745=DIRECTION('',(0.,0.,1.));
#10746=DIRECTION('',(0.,0.,1.));
#10747=DIRECTION('',(1.,0.,0.));
#10748=DIRECTION('center_axis',(0.,0.56333682464151,0.826227342807548));
#10749=DIRECTION('ref_axis',(0.,-0.826227342807548,0.56333682464151));
#10750=DIRECTION('',(0.,-0.826227342807548,0.56333682464151));
#10751=DIRECTION('',(0.,-0.826227342807548,0.56333682464151));
#10752=DIRECTION('',(1.,0.,0.));
#10753=DIRECTION('center_axis',(0.,1.,0.));
#10754=DIRECTION('ref_axis',(0.,0.,1.));
#10755=DIRECTION('',(0.,0.,1.));
#10756=DIRECTION('',(0.,0.,1.));
#10757=DIRECTION('',(1.,0.,0.));
#10758=DIRECTION('center_axis',(0.,0.,-1.));
#10759=DIRECTION('ref_axis',(0.,1.,0.));
#10760=DIRECTION('',(0.,1.,0.));
#10761=DIRECTION('',(0.,1.,0.));
#10762=DIRECTION('',(1.,0.,0.));
#10763=DIRECTION('center_axis',(0.,-1.,0.));
#10764=DIRECTION('ref_axis',(0.,0.,-1.));
#10765=DIRECTION('',(0.,0.,-1.));
#10766=DIRECTION('',(0.,0.,-1.));
#10767=DIRECTION('center_axis',(1.,0.,0.));
#10768=DIRECTION('ref_axis',(0.,0.,-1.));
#10769=DIRECTION('center_axis',(1.,0.,0.));
#10770=DIRECTION('ref_axis',(0.,0.,-1.));
#10771=DIRECTION('axis',(0.,0.,1.));
#10772=DIRECTION('refdir',(1.,0.,0.));
#10773=DIRECTION('center_axis',(0.,0.,-1.));
#10774=DIRECTION('ref_axis',(0.,1.,0.));
#10775=DIRECTION('',(0.,1.,0.));
#10776=DIRECTION('',(1.,0.,0.));
#10777=DIRECTION('',(0.,-1.,0.));
#10778=DIRECTION('',(1.,0.,0.));
#10779=DIRECTION('center_axis',(0.,1.,-8.88178419700125E-16));
#10780=DIRECTION('ref_axis',(0.,8.88178419700125E-16,1.));
#10781=DIRECTION('',(0.,8.88178419700125E-16,1.));
#10782=DIRECTION('',(1.,0.,0.));
#10783=DIRECTION('',(0.,-8.88178419700125E-16,-1.));
#10784=DIRECTION('center_axis',(0.,-7.40148683083439E-16,-1.));
#10785=DIRECTION('ref_axis',(0.,1.,-7.40148683083439E-16));
#10786=DIRECTION('',(0.,1.,-7.40148683083439E-16));
#10787=DIRECTION('',(1.,0.,0.));
#10788=DIRECTION('',(0.,-1.,7.40148683083439E-16));
#10789=DIRECTION('center_axis',(0.,-0.707106781186547,-0.707106781186548));
#10790=DIRECTION('ref_axis',(0.,0.707106781186548,-0.707106781186547));
#10791=DIRECTION('',(0.,0.707106781186548,-0.707106781186547));
#10792=DIRECTION('',(1.,0.,0.));
#10793=DIRECTION('',(0.,-0.707106781186548,0.707106781186547));
#10794=DIRECTION('center_axis',(0.,-1.,2.77555756156289E-16));
#10795=DIRECTION('ref_axis',(0.,-2.77555756156289E-16,-1.));
#10796=DIRECTION('',(0.,-2.77555756156289E-16,-1.));
#10797=DIRECTION('',(1.,0.,0.));
#10798=DIRECTION('',(0.,2.77555756156289E-16,1.));
#10799=DIRECTION('center_axis',(0.,-0.707106781186547,0.707106781186548));
#10800=DIRECTION('ref_axis',(0.,-0.707106781186548,-0.707106781186547));
#10801=DIRECTION('',(0.,-0.707106781186548,-0.707106781186547));
#10802=DIRECTION('',(1.,0.,0.));
#10803=DIRECTION('',(0.,0.707106781186548,0.707106781186547));
#10804=DIRECTION('center_axis',(0.,7.40148683083438E-16,1.));
#10805=DIRECTION('ref_axis',(0.,-1.,7.40148683083438E-16));
#10806=DIRECTION('',(0.,-1.,7.40148683083438E-16));
#10807=DIRECTION('',(1.,0.,0.));
#10808=DIRECTION('',(0.,1.,-7.40148683083438E-16));
#10809=DIRECTION('center_axis',(0.,1.,-4.44089209850063E-16));
#10810=DIRECTION('ref_axis',(0.,4.44089209850063E-16,1.));
#10811=DIRECTION('',(0.,4.44089209850063E-16,1.));
#10812=DIRECTION('',(1.,0.,0.));
#10813=DIRECTION('',(0.,-4.44089209850063E-16,-1.));
#10814=DIRECTION('center_axis',(0.,2.41352831440251E-16,1.));
#10815=DIRECTION('ref_axis',(0.,-1.,2.41352831440251E-16));
#10816=DIRECTION('',(0.,-1.,2.41352831440251E-16));
#10817=DIRECTION('',(-1.,0.,0.));
#10818=DIRECTION('',(0.,1.,-2.41352831440251E-16));
#10819=DIRECTION('center_axis',(0.,-1.,2.41352831440251E-16));
#10820=DIRECTION('ref_axis',(0.,-2.41352831440251E-16,-1.));
#10821=DIRECTION('',(0.,-2.41352831440251E-16,-1.));
#10822=DIRECTION('',(1.,0.,0.));
#10823=DIRECTION('',(0.,2.41352831440251E-16,1.));
#10824=DIRECTION('',(1.,0.,0.));
#10825=DIRECTION('center_axis',(0.,0.,-1.));
#10826=DIRECTION('ref_axis',(0.,1.,0.));
#10827=DIRECTION('',(0.,1.,0.));
#10828=DIRECTION('',(1.,0.,0.));
#10829=DIRECTION('',(0.,-1.,0.));
#10830=DIRECTION('center_axis',(0.,-1.,0.));
#10831=DIRECTION('ref_axis',(0.,0.,-1.));
#10832=DIRECTION('',(0.,0.,-1.));
#10833=DIRECTION('',(1.,0.,0.));
#10834=DIRECTION('',(0.,0.,1.));
#10835=DIRECTION('center_axis',(0.,-0.707106781186547,0.707106781186548));
#10836=DIRECTION('ref_axis',(0.,-0.707106781186548,-0.707106781186547));
#10837=DIRECTION('',(0.,-0.707106781186548,-0.707106781186547));
#10838=DIRECTION('',(1.,0.,0.));
#10839=DIRECTION('',(0.,0.707106781186548,0.707106781186547));
#10840=DIRECTION('center_axis',(0.,0.,1.));
#10841=DIRECTION('ref_axis',(0.,-1.,0.));
#10842=DIRECTION('',(0.,-1.,0.));
#10843=DIRECTION('',(1.,0.,0.));
#10844=DIRECTION('',(0.,1.,0.));
#10845=DIRECTION('center_axis',(0.,0.707106781186548,0.707106781186547));
#10846=DIRECTION('ref_axis',(0.,-0.707106781186547,0.707106781186548));
#10847=DIRECTION('',(0.,-0.707106781186547,0.707106781186548));
#10848=DIRECTION('',(1.,0.,0.));
#10849=DIRECTION('',(0.,0.707106781186547,-0.707106781186548));
#10850=DIRECTION('center_axis',(0.,1.,0.));
#10851=DIRECTION('ref_axis',(0.,0.,1.));
#10852=DIRECTION('',(0.,0.,1.));
#10853=DIRECTION('',(1.,0.,0.));
#10854=DIRECTION('',(0.,0.,-1.));
#10855=DIRECTION('center_axis',(0.,0.,-1.));
#10856=DIRECTION('ref_axis',(0.,1.,0.));
#10857=DIRECTION('',(0.,1.,0.));
#10858=DIRECTION('',(1.,0.,0.));
#10859=DIRECTION('',(0.,-1.,0.));
#10860=DIRECTION('center_axis',(0.,1.,-2.41352831440251E-16));
#10861=DIRECTION('ref_axis',(0.,2.41352831440251E-16,1.));
#10862=DIRECTION('',(0.,2.41352831440251E-16,1.));
#10863=DIRECTION('',(-1.,0.,0.));
#10864=DIRECTION('',(0.,-2.41352831440251E-16,-1.));
#10865=DIRECTION('center_axis',(0.,0.,1.));
#10866=DIRECTION('ref_axis',(0.,-1.,0.));
#10867=DIRECTION('',(0.,-1.,0.));
#10868=DIRECTION('',(1.,0.,0.));
#10869=DIRECTION('',(0.,1.,0.));
#10870=DIRECTION('',(1.,0.,0.));
#10871=DIRECTION('center_axis',(0.,-1.,0.));
#10872=DIRECTION('ref_axis',(0.,0.,-1.));
#10873=DIRECTION('',(0.,0.,-1.));
#10874=DIRECTION('',(1.,0.,0.));
#10875=DIRECTION('',(0.,0.,1.));
#10876=DIRECTION('center_axis',(0.,0.,1.));
#10877=DIRECTION('ref_axis',(0.,-1.,0.));
#10878=DIRECTION('',(0.,-1.,0.));
#10879=DIRECTION('',(1.,0.,0.));
#10880=DIRECTION('',(0.,1.,0.));
#10881=DIRECTION('center_axis',(0.,0.707106781186548,0.707106781186548));
#10882=DIRECTION('ref_axis',(0.,-0.707106781186548,0.707106781186548));
#10883=DIRECTION('',(0.,-0.707106781186548,0.707106781186548));
#10884=DIRECTION('',(1.,0.,0.));
#10885=DIRECTION('',(0.,0.707106781186548,-0.707106781186548));
#10886=DIRECTION('center_axis',(0.,1.,0.));
#10887=DIRECTION('ref_axis',(0.,0.,1.));
#10888=DIRECTION('',(0.,0.,1.));
#10889=DIRECTION('',(1.,0.,0.));
#10890=DIRECTION('',(0.,0.,-1.));
#10891=DIRECTION('center_axis',(0.,0.707106781186548,-0.707106781186547));
#10892=DIRECTION('ref_axis',(0.,0.707106781186547,0.707106781186548));
#10893=DIRECTION('',(0.,0.707106781186547,0.707106781186548));
#10894=DIRECTION('',(1.,0.,0.));
#10895=DIRECTION('',(0.,-0.707106781186547,-0.707106781186548));
#10896=DIRECTION('center_axis',(0.,-7.40148683083438E-16,-1.));
#10897=DIRECTION('ref_axis',(0.,1.,-7.40148683083438E-16));
#10898=DIRECTION('',(0.,1.,-7.40148683083438E-16));
#10899=DIRECTION('',(1.,0.,0.));
#10900=DIRECTION('',(0.,-1.,7.40148683083438E-16));
#10901=DIRECTION('center_axis',(0.,-1.,0.));
#10902=DIRECTION('ref_axis',(0.,0.,-1.));
#10903=DIRECTION('',(0.,0.,-1.));
#10904=DIRECTION('',(1.,0.,0.));
#10905=DIRECTION('',(0.,0.,1.));
#10906=DIRECTION('center_axis',(0.,0.,-1.));
#10907=DIRECTION('ref_axis',(0.,1.,0.));
#10908=DIRECTION('',(0.,1.,0.));
#10909=DIRECTION('',(-1.,0.,0.));
#10910=DIRECTION('',(0.,-1.,0.));
#10911=DIRECTION('center_axis',(0.,1.,0.));
#10912=DIRECTION('ref_axis',(0.,0.,1.));
#10913=DIRECTION('',(0.,0.,1.));
#10914=DIRECTION('',(1.,0.,0.));
#10915=DIRECTION('',(0.,0.,-1.));
#10916=DIRECTION('',(1.,0.,0.));
#10917=DIRECTION('center_axis',(0.,0.,1.));
#10918=DIRECTION('ref_axis',(0.,-1.,0.));
#10919=DIRECTION('',(0.,-1.,0.));
#10920=DIRECTION('',(1.,0.,0.));
#10921=DIRECTION('',(0.,1.,0.));
#10922=DIRECTION('center_axis',(0.,1.,0.));
#10923=DIRECTION('ref_axis',(0.,0.,1.));
#10924=DIRECTION('',(0.,0.,1.));
#10925=DIRECTION('',(1.,0.,0.));
#10926=DIRECTION('',(0.,0.,-1.));
#10927=DIRECTION('center_axis',(0.,0.707106781186547,-0.707106781186548));
#10928=DIRECTION('ref_axis',(0.,0.707106781186548,0.707106781186547));
#10929=DIRECTION('',(0.,0.707106781186548,0.707106781186547));
#10930=DIRECTION('',(1.,0.,0.));
#10931=DIRECTION('',(0.,-0.707106781186548,-0.707106781186547));
#10932=DIRECTION('center_axis',(0.,0.,-1.));
#10933=DIRECTION('ref_axis',(0.,1.,0.));
#10934=DIRECTION('',(0.,1.,0.));
#10935=DIRECTION('',(1.,0.,0.));
#10936=DIRECTION('',(0.,-1.,0.));
#10937=DIRECTION('center_axis',(0.,-0.707106781186547,-0.707106781186548));
#10938=DIRECTION('ref_axis',(0.,0.707106781186548,-0.707106781186547));
#10939=DIRECTION('',(0.,0.707106781186548,-0.707106781186547));
#10940=DIRECTION('',(1.,0.,0.));
#10941=DIRECTION('',(0.,-0.707106781186548,0.707106781186547));
#10942=DIRECTION('center_axis',(0.,-1.,0.));
#10943=DIRECTION('ref_axis',(0.,0.,-1.));
#10944=DIRECTION('',(0.,0.,-1.));
#10945=DIRECTION('',(1.,0.,0.));
#10946=DIRECTION('',(0.,0.,1.));
#10947=DIRECTION('center_axis',(0.,0.,1.));
#10948=DIRECTION('ref_axis',(0.,-1.,0.));
#10949=DIRECTION('',(0.,-1.,0.));
#10950=DIRECTION('',(1.,0.,0.));
#10951=DIRECTION('',(0.,1.,0.));
#10952=DIRECTION('center_axis',(0.,-1.,0.));
#10953=DIRECTION('ref_axis',(0.,0.,-1.));
#10954=DIRECTION('',(0.,0.,-1.));
#10955=DIRECTION('',(-1.,0.,0.));
#10956=DIRECTION('',(0.,0.,1.));
#10957=DIRECTION('center_axis',(1.,0.,0.));
#10958=DIRECTION('ref_axis',(0.,0.,-1.));
#10959=DIRECTION('center_axis',(1.,0.,0.));
#10960=DIRECTION('ref_axis',(0.,0.,-1.));
#10961=DIRECTION('',(1.,0.,0.));
#10962=DIRECTION('center_axis',(-1.,0.,0.));
#10963=DIRECTION('ref_axis',(0.,0.,-1.));
#10964=DIRECTION('center_axis',(0.,1.,0.));
#10965=DIRECTION('ref_axis',(0.,0.,1.));
#10966=DIRECTION('',(0.,0.,1.));
#10967=DIRECTION('',(1.,0.,0.));
#10968=DIRECTION('',(0.,0.,1.));
#10969=DIRECTION('center_axis',(0.,1.,0.));
#10970=DIRECTION('ref_axis',(0.,0.,1.));
#10971=DIRECTION('',(0.,0.,1.));
#10972=DIRECTION('',(1.,0.,0.));
#10973=DIRECTION('',(0.,0.,1.));
#10974=DIRECTION('center_axis',(0.,0.,-1.));
#10975=DIRECTION('ref_axis',(0.,1.,0.));
#10976=DIRECTION('',(0.,1.,0.));
#10977=DIRECTION('',(0.,1.,0.));
#10978=DIRECTION('center_axis',(0.,0.,-1.));
#10979=DIRECTION('ref_axis',(0.,1.,0.));
#10980=DIRECTION('',(0.,1.,0.));
#10981=DIRECTION('',(1.,0.,0.));
#10982=DIRECTION('',(0.,1.,0.));
#10983=DIRECTION('center_axis',(0.,-1.,0.));
#10984=DIRECTION('ref_axis',(0.,0.,-1.));
#10985=DIRECTION('',(0.,0.,-1.));
#10986=DIRECTION('',(0.,0.,-1.));
#10987=DIRECTION('center_axis',(0.,-1.,0.));
#10988=DIRECTION('ref_axis',(0.,0.,-1.));
#10989=DIRECTION('',(0.,0.,-1.));
#10990=DIRECTION('',(1.,0.,0.));
#10991=DIRECTION('',(0.,0.,-1.));
#10992=DIRECTION('center_axis',(0.,0.,1.));
#10993=DIRECTION('ref_axis',(0.,-1.,0.));
#10994=DIRECTION('',(0.,-1.,0.));
#10995=DIRECTION('',(0.,-1.,0.));
#10996=DIRECTION('center_axis',(0.,0.,1.));
#10997=DIRECTION('ref_axis',(0.,-1.,0.));
#10998=DIRECTION('',(0.,-1.,0.));
#10999=DIRECTION('',(0.,-1.,0.));
#11000=DIRECTION('center_axis',(1.,0.,0.));
#11001=DIRECTION('ref_axis',(0.,0.,-1.));
#11002=DIRECTION('center_axis',(1.,0.,0.));
#11003=DIRECTION('ref_axis',(0.,0.,-1.));
#11004=DIRECTION('axis',(0.,0.,1.));
#11005=DIRECTION('refdir',(1.,0.,0.));
#11006=DIRECTION('center_axis',(0.,0.,1.));
#11007=DIRECTION('ref_axis',(1.,0.,0.));
#11008=DIRECTION('',(1.,0.,0.));
#11009=DIRECTION('',(0.,-1.,0.));
#11010=DIRECTION('',(-1.,0.,0.));
#11011=DIRECTION('',(0.,1.,0.));
#11012=DIRECTION('center_axis',(0.,1.,0.));
#11013=DIRECTION('ref_axis',(-1.,0.,0.));
#11014=DIRECTION('',(0.,0.,1.));
#11015=DIRECTION('',(-1.,0.,0.));
#11016=DIRECTION('',(0.,0.,1.));
#11017=DIRECTION('center_axis',(0.,0.,1.));
#11018=DIRECTION('ref_axis',(1.,0.,0.));
#11019=DIRECTION('',(0.,-1.,0.));
#11020=DIRECTION('',(1.,0.,0.));
#11021=DIRECTION('',(0.,1.,0.));
#11022=DIRECTION('center_axis',(0.,0.,-1.));
#11023=DIRECTION('ref_axis',(1.,0.,0.));
#11024=DIRECTION('center_axis',(-1.,0.,0.));
#11025=DIRECTION('ref_axis',(0.,-1.,0.));
#11026=DIRECTION('',(0.,0.,1.));
#11027=DIRECTION('',(0.,0.707106781186548,0.707106781186548));
#11028=DIRECTION('',(0.,-1.,0.));
#11029=DIRECTION('',(0.,0.707106781186548,-0.707106781186548));
#11030=DIRECTION('',(0.,0.,1.));
#11031=DIRECTION('',(0.,-1.,0.));
#11032=DIRECTION('',(0.,0.,1.));
#11033=DIRECTION('center_axis',(0.,-1.,0.));
#11034=DIRECTION('ref_axis',(1.,0.,0.));
#11035=DIRECTION('',(1.,0.,0.));
#11036=DIRECTION('',(0.,0.,1.));
#11037=DIRECTION('center_axis',(0.,0.,1.));
#11038=DIRECTION('ref_axis',(1.,0.,0.));
#11039=DIRECTION('',(-1.,0.,0.));
#11040=DIRECTION('',(0.,1.,0.));
#11041=DIRECTION('center_axis',(1.,0.,0.));
#11042=DIRECTION('ref_axis',(0.,1.,0.));
#11043=DIRECTION('',(0.,0.,1.));
#11044=DIRECTION('',(0.,-0.707106781186548,0.707106781186548));
#11045=DIRECTION('',(0.,1.,0.));
#11046=DIRECTION('',(0.,-0.707106781186548,-0.707106781186548));
#11047=DIRECTION('',(0.,0.,1.));
#11048=DIRECTION('center_axis',(0.,-1.,0.));
#11049=DIRECTION('ref_axis',(1.,0.,0.));
#11050=DIRECTION('',(-1.,0.,0.));
#11051=DIRECTION('center_axis',(0.,-0.707106781186548,-0.707106781186548));
#11052=DIRECTION('ref_axis',(-1.,0.,0.));
#11053=DIRECTION('',(1.,0.,0.));
#11054=DIRECTION('center_axis',(0.,0.707106781186548,0.707106781186548));
#11055=DIRECTION('ref_axis',(0.,0.707106781186547,-0.707106781186547));
#11056=DIRECTION('',(1.,0.,0.));
#11057=DIRECTION('center_axis',(0.,0.,1.));
#11058=DIRECTION('ref_axis',(1.,0.,0.));
#11059=DIRECTION('center_axis',(0.,0.,-1.));
#11060=DIRECTION('ref_axis',(1.,0.,0.));
#11061=DIRECTION('',(0.,0.,1.));
#11062=DIRECTION('center_axis',(0.,0.,-1.));
#11063=DIRECTION('ref_axis',(1.,0.,0.));
#11064=DIRECTION('center_axis',(0.,-0.707106781186548,0.707106781186548));
#11065=DIRECTION('ref_axis',(0.,0.707106781186547,0.707106781186547));
#11066=DIRECTION('center_axis',(0.,0.,-1.));
#11067=DIRECTION('ref_axis',(1.,0.,0.));
#11068=DIRECTION('center_axis',(0.,0.,1.));
#11069=DIRECTION('ref_axis',(1.,0.,0.));
#11070=DIRECTION('',(-1.,0.,0.));
#11071=DIRECTION('center_axis',(0.,0.,1.));
#11072=DIRECTION('ref_axis',(1.,0.,0.));
#11073=DIRECTION('',(-1.,0.,0.));
#11074=DIRECTION('center_axis',(0.,0.707106781186548,-0.707106781186548));
#11075=DIRECTION('ref_axis',(-1.,0.,0.));
#11076=DIRECTION('',(1.,0.,0.));
#11077=DIRECTION('center_axis',(0.,1.,0.));
#11078=DIRECTION('ref_axis',(-1.,0.,0.));
#11079=DIRECTION('axis',(0.,0.,1.));
#11080=DIRECTION('refdir',(1.,0.,0.));
#11081=DIRECTION('center_axis',(0.866025403784439,0.,-0.5));
#11082=DIRECTION('ref_axis',(0.5,0.,0.866025403784439));
#11083=DIRECTION('',(-0.5,0.,-0.866025403784439));
#11084=DIRECTION('',(0.,-1.,0.));
#11085=DIRECTION('',(0.5,0.,0.866025403784439));
#11086=DIRECTION('',(0.,-1.,0.));
#11087=DIRECTION('center_axis',(1.20185167898973E-16,0.,-1.));
#11088=DIRECTION('ref_axis',(1.,0.,1.20185167898973E-16));
#11089=DIRECTION('',(-1.,0.,-1.20185167898973E-16));
#11090=DIRECTION('',(0.,-1.,0.));
#11091=DIRECTION('',(1.,0.,1.20185167898973E-16));
#11092=DIRECTION('center_axis',(-0.866025403784439,0.,-0.5));
#11093=DIRECTION('ref_axis',(0.5,0.,-0.866025403784439));
#11094=DIRECTION('',(-0.5,0.,0.866025403784439));
#11095=DIRECTION('',(0.,-1.,0.));
#11096=DIRECTION('',(0.5,0.,-0.866025403784439));
#11097=DIRECTION('center_axis',(-0.866025403784439,0.,0.5));
#11098=DIRECTION('ref_axis',(-0.5,0.,-0.866025403784439));
#11099=DIRECTION('',(0.5,0.,0.866025403784439));
#11100=DIRECTION('',(0.,-1.,0.));
#11101=DIRECTION('',(-0.5,0.,-0.866025403784439));
#11102=DIRECTION('center_axis',(-2.40370335797945E-16,0.,1.));
#11103=DIRECTION('ref_axis',(-1.,0.,-2.40370335797945E-16));
#11104=DIRECTION('',(1.,0.,2.40370335797945E-16));
#11105=DIRECTION('',(0.,-1.,0.));
#11106=DIRECTION('',(-1.,0.,-2.40370335797945E-16));
#11107=DIRECTION('center_axis',(0.866025403784439,0.,0.5));
#11108=DIRECTION('ref_axis',(-0.5,0.,0.866025403784439));
#11109=DIRECTION('',(0.5,0.,-0.866025403784439));
#11110=DIRECTION('',(-0.5,0.,0.866025403784439));
#11111=DIRECTION('center_axis',(0.,1.,0.));
#11112=DIRECTION('ref_axis',(1.,0.,0.));
#11113=DIRECTION('center_axis',(0.,-1.,0.));
#11114=DIRECTION('ref_axis',(0.,0.,-1.));
#11115=DIRECTION('center_axis',(0.,1.,0.));
#11116=DIRECTION('ref_axis',(1.,0.,0.));
#11117=DIRECTION('center_axis',(0.,1.,0.));
#11118=DIRECTION('ref_axis',(1.,0.,0.));
#11119=DIRECTION('center_axis',(0.,1.,0.));
#11120=DIRECTION('ref_axis',(0.,0.,1.));
#11121=DIRECTION('center_axis',(0.,-1.,0.));
#11122=DIRECTION('ref_axis',(1.,0.,0.));
#11123=DIRECTION('center_axis',(0.,-1.,0.));
#11124=DIRECTION('ref_axis',(1.,0.,0.));
#11125=DIRECTION('center_axis',(0.,-1.,0.));
#11126=DIRECTION('ref_axis',(1.,0.,0.));
#11127=DIRECTION('',(0.707106781186548,0.707106781186547,8.65956056235493E-17));
#11128=DIRECTION('center_axis',(0.,-1.,0.));
#11129=DIRECTION('ref_axis',(1.,0.,0.));
#11130=DIRECTION('center_axis',(0.,-1.,0.));
#11131=DIRECTION('ref_axis',(1.,0.,0.));
#11132=DIRECTION('',(0.,1.,0.));
#11133=DIRECTION('center_axis',(0.,1.,0.));
#11134=DIRECTION('ref_axis',(1.,0.,0.));
#11135=DIRECTION('center_axis',(0.,-1.,0.));
#11136=DIRECTION('ref_axis',(1.,0.,0.));
#11137=DIRECTION('',(-0.707106781186547,0.707106781186548,-8.65956056235493E-17));
#11138=DIRECTION('center_axis',(0.,-1.,0.));
#11139=DIRECTION('ref_axis',(0.,0.,-1.));
#11140=DIRECTION('center_axis',(0.,-1.,0.));
#11141=DIRECTION('ref_axis',(1.,0.,0.));
#11142=DIRECTION('center_axis',(0.,1.,0.));
#11143=DIRECTION('ref_axis',(1.,0.,0.));
#11144=DIRECTION('center_axis',(0.,1.,0.));
#11145=DIRECTION('ref_axis',(1.,0.,0.));
#11146=DIRECTION('',(-0.447213595499958,0.894427190999916,-5.47678698264203E-17));
#11147=DIRECTION('center_axis',(0.,-1.,0.));
#11148=DIRECTION('ref_axis',(1.,0.,0.));
#11149=DIRECTION('',(0.,1.,0.));
#11150=DIRECTION('axis',(0.,0.,1.));
#11151=DIRECTION('refdir',(1.,0.,0.));
#11152=DIRECTION('center_axis',(0.866025403784439,0.,-0.5));
#11153=DIRECTION('ref_axis',(0.5,0.,0.866025403784439));
#11154=DIRECTION('',(-0.5,0.,-0.866025403784439));
#11155=DIRECTION('',(0.,-1.,0.));
#11156=DIRECTION('',(0.5,0.,0.866025403784439));
#11157=DIRECTION('',(0.,-1.,0.));
#11158=DIRECTION('center_axis',(1.60246890531964E-16,0.,-1.));
#11159=DIRECTION('ref_axis',(1.,0.,1.60246890531964E-16));
#11160=DIRECTION('',(-1.,0.,-1.60246890531964E-16));
#11161=DIRECTION('',(0.,-1.,0.));
#11162=DIRECTION('',(1.,0.,1.60246890531964E-16));
#11163=DIRECTION('center_axis',(-0.866025403784439,0.,-0.5));
#11164=DIRECTION('ref_axis',(0.5,0.,-0.866025403784439));
#11165=DIRECTION('',(-0.5,0.,0.866025403784439));
#11166=DIRECTION('',(0.,-1.,0.));
#11167=DIRECTION('',(0.5,0.,-0.866025403784439));
#11168=DIRECTION('center_axis',(-0.866025403784439,0.,0.5));
#11169=DIRECTION('ref_axis',(-0.5,0.,-0.866025403784439));
#11170=DIRECTION('',(0.5,0.,0.866025403784439));
#11171=DIRECTION('',(0.,-1.,0.));
#11172=DIRECTION('',(-0.5,0.,-0.866025403784439));
#11173=DIRECTION('center_axis',(-1.60246890531964E-16,0.,1.));
#11174=DIRECTION('ref_axis',(-1.,0.,-1.60246890531964E-16));
#11175=DIRECTION('',(1.,0.,1.60246890531964E-16));
#11176=DIRECTION('',(0.,-1.,0.));
#11177=DIRECTION('',(-1.,0.,-1.60246890531964E-16));
#11178=DIRECTION('center_axis',(0.866025403784439,0.,0.5));
#11179=DIRECTION('ref_axis',(-0.5,0.,0.866025403784439));
#11180=DIRECTION('',(0.5,0.,-0.866025403784439));
#11181=DIRECTION('',(-0.5,0.,0.866025403784439));
#11182=DIRECTION('center_axis',(0.,1.,0.));
#11183=DIRECTION('ref_axis',(1.,0.,0.));
#11184=DIRECTION('center_axis',(0.,-1.,0.));
#11185=DIRECTION('ref_axis',(0.,0.,-1.));
#11186=DIRECTION('center_axis',(0.,1.,0.));
#11187=DIRECTION('ref_axis',(1.,0.,0.));
#11188=DIRECTION('center_axis',(0.,1.,0.));
#11189=DIRECTION('ref_axis',(1.,0.,0.));
#11190=DIRECTION('center_axis',(0.,1.,0.));
#11191=DIRECTION('ref_axis',(0.,0.,1.));
#11192=DIRECTION('center_axis',(0.,-1.,0.));
#11193=DIRECTION('ref_axis',(1.,0.,0.));
#11194=DIRECTION('center_axis',(0.,-1.,0.));
#11195=DIRECTION('ref_axis',(1.,0.,0.));
#11196=DIRECTION('center_axis',(0.,-1.,0.));
#11197=DIRECTION('ref_axis',(1.,0.,0.));
#11198=DIRECTION('',(0.707106781186547,0.707106781186548,8.65956056235493E-17));
#11199=DIRECTION('center_axis',(0.,-1.,0.));
#11200=DIRECTION('ref_axis',(1.,0.,0.));
#11201=DIRECTION('center_axis',(0.,-1.,0.));
#11202=DIRECTION('ref_axis',(1.,0.,0.));
#11203=DIRECTION('',(0.,1.,0.));
#11204=DIRECTION('center_axis',(0.,1.,0.));
#11205=DIRECTION('ref_axis',(1.,0.,0.));
#11206=DIRECTION('center_axis',(0.,-1.,0.));
#11207=DIRECTION('ref_axis',(1.,0.,0.));
#11208=DIRECTION('',(-0.707106781186547,0.707106781186548,-8.65956056235493E-17));
#11209=DIRECTION('center_axis',(0.,-1.,0.));
#11210=DIRECTION('ref_axis',(0.,0.,-1.));
#11211=DIRECTION('center_axis',(0.,-1.,0.));
#11212=DIRECTION('ref_axis',(1.,0.,0.));
#11213=DIRECTION('center_axis',(0.,1.,0.));
#11214=DIRECTION('ref_axis',(1.,0.,0.));
#11215=DIRECTION('center_axis',(0.,1.,0.));
#11216=DIRECTION('ref_axis',(1.,0.,0.));
#11217=DIRECTION('',(-0.447213595499958,0.894427190999916,-5.47678698264203E-17));
#11218=DIRECTION('center_axis',(0.,-1.,0.));
#11219=DIRECTION('ref_axis',(1.,0.,0.));
#11220=DIRECTION('',(0.,1.,0.));
#11221=DIRECTION('axis',(0.,0.,1.));
#11222=DIRECTION('refdir',(1.,0.,0.));
#11223=DIRECTION('axis',(0.,0.,1.));
#11224=DIRECTION('refdir',(1.,0.,0.));
#11225=DIRECTION('center_axis',(0.,0.,1.));
#11226=DIRECTION('ref_axis',(1.,0.,0.));
#11227=DIRECTION('center_axis',(0.,0.,1.));
#11228=DIRECTION('ref_axis',(1.,0.,0.));
#11229=DIRECTION('',(0.,0.,1.));
#11230=DIRECTION('center_axis',(0.,0.,-1.));
#11231=DIRECTION('ref_axis',(1.,0.,0.));
#11232=DIRECTION('center_axis',(0.,0.,1.));
#11233=DIRECTION('ref_axis',(1.,0.,0.));
#11234=DIRECTION('center_axis',(0.,0.,1.));
#11235=DIRECTION('ref_axis',(1.,0.,0.));
#11236=DIRECTION('',(0.,0.,1.));
#11237=DIRECTION('center_axis',(0.,0.,-1.));
#11238=DIRECTION('ref_axis',(1.,0.,0.));
#11239=DIRECTION('center_axis',(0.,0.,1.));
#11240=DIRECTION('ref_axis',(1.,0.,0.));
#11241=DIRECTION('center_axis',(0.,0.,1.));
#11242=DIRECTION('ref_axis',(1.,0.,0.));
#11243=DIRECTION('',(0.,0.,1.));
#11244=DIRECTION('center_axis',(0.,0.,-1.));
#11245=DIRECTION('ref_axis',(1.,0.,0.));
#11246=DIRECTION('center_axis',(0.,0.,1.));
#11247=DIRECTION('ref_axis',(1.,0.,0.));
#11248=DIRECTION('center_axis',(0.,0.,1.));
#11249=DIRECTION('ref_axis',(1.,0.,0.));
#11250=DIRECTION('',(0.,0.,1.));
#11251=DIRECTION('center_axis',(0.,0.,-1.));
#11252=DIRECTION('ref_axis',(1.,0.,0.));
#11253=DIRECTION('center_axis',(0.,0.,1.));
#11254=DIRECTION('ref_axis',(1.,0.,0.));
#11255=DIRECTION('center_axis',(0.,0.,1.));
#11256=DIRECTION('ref_axis',(1.,0.,0.));
#11257=DIRECTION('',(0.,0.,1.));
#11258=DIRECTION('center_axis',(0.,0.,-1.));
#11259=DIRECTION('ref_axis',(1.,0.,0.));
#11260=DIRECTION('center_axis',(0.,0.,1.));
#11261=DIRECTION('ref_axis',(1.,0.,0.));
#11262=DIRECTION('center_axis',(0.,0.,1.));
#11263=DIRECTION('ref_axis',(1.,0.,0.));
#11264=DIRECTION('',(0.,0.,1.));
#11265=DIRECTION('center_axis',(0.,0.,-1.));
#11266=DIRECTION('ref_axis',(1.,0.,0.));
#11267=DIRECTION('center_axis',(0.,1.,0.));
#11268=DIRECTION('ref_axis',(-1.,0.,0.));
#11269=DIRECTION('',(-1.,0.,0.));
#11270=DIRECTION('',(0.,0.,1.));
#11271=DIRECTION('',(-1.,0.,0.));
#11272=DIRECTION('',(0.,0.,1.));
#11273=DIRECTION('center_axis',(1.,0.,0.));
#11274=DIRECTION('ref_axis',(0.,1.,0.));
#11275=DIRECTION('',(0.,1.,0.));
#11276=DIRECTION('',(0.,1.,0.));
#11277=DIRECTION('',(0.,0.,1.));
#11278=DIRECTION('center_axis',(0.,-1.,0.));
#11279=DIRECTION('ref_axis',(1.,0.,0.));
#11280=DIRECTION('',(1.,0.,0.));
#11281=DIRECTION('',(1.,0.,0.));
#11282=DIRECTION('',(0.,0.,1.));
#11283=DIRECTION('center_axis',(-1.,0.,0.));
#11284=DIRECTION('ref_axis',(0.,-1.,0.));
#11285=DIRECTION('',(0.,-1.,0.));
#11286=DIRECTION('',(0.,-1.,0.));
#11287=DIRECTION('center_axis',(0.,0.,1.));
#11288=DIRECTION('ref_axis',(1.,0.,0.));
#11289=DIRECTION('center_axis',(0.,0.,1.));
#11290=DIRECTION('ref_axis',(1.,0.,0.));
#11291=DIRECTION('axis',(0.,0.,1.));
#11292=DIRECTION('refdir',(1.,0.,0.));
#11293=DIRECTION('center_axis',(0.,0.,1.));
#11294=DIRECTION('ref_axis',(1.,0.,0.));
#11295=DIRECTION('center_axis',(0.,0.,1.));
#11296=DIRECTION('ref_axis',(1.,0.,0.));
#11297=DIRECTION('',(0.,0.,1.));
#11298=DIRECTION('center_axis',(0.,0.,-1.));
#11299=DIRECTION('ref_axis',(1.,0.,0.));
#11300=DIRECTION('center_axis',(0.,0.,1.));
#11301=DIRECTION('ref_axis',(0.,-1.,0.));
#11302=DIRECTION('',(0.,-1.,0.));
#11303=DIRECTION('',(1.,0.,0.));
#11304=DIRECTION('',(0.,-1.,0.));
#11305=DIRECTION('',(1.,0.,0.));
#11306=DIRECTION('center_axis',(0.,1.,0.));
#11307=DIRECTION('ref_axis',(0.,0.,1.));
#11308=DIRECTION('',(0.,0.,1.));
#11309=DIRECTION('',(0.,0.,1.));
#11310=DIRECTION('',(1.,0.,0.));
#11311=DIRECTION('center_axis',(0.,0.,-1.));
#11312=DIRECTION('ref_axis',(0.,1.,0.));
#11313=DIRECTION('',(0.,1.,0.));
#11314=DIRECTION('',(0.,1.,0.));
#11315=DIRECTION('',(1.,0.,0.));
#11316=DIRECTION('center_axis',(0.,-1.,0.));
#11317=DIRECTION('ref_axis',(0.,0.,-1.));
#11318=DIRECTION('',(0.,0.,-1.));
#11319=DIRECTION('',(0.,0.,-1.));
#11320=DIRECTION('',(1.,0.,0.));
#11321=DIRECTION('center_axis',(0.,0.,-1.));
#11322=DIRECTION('ref_axis',(0.,1.,0.));
#11323=DIRECTION('',(0.,1.,0.));
#11324=DIRECTION('',(0.,1.,0.));
#11325=DIRECTION('',(1.,0.,0.));
#11326=DIRECTION('center_axis',(0.,-1.,0.));
#11327=DIRECTION('ref_axis',(0.,0.,-1.));
#11328=DIRECTION('',(0.,0.,-1.));
#11329=DIRECTION('',(0.,0.,-1.));
#11330=DIRECTION('center_axis',(1.,0.,0.));
#11331=DIRECTION('ref_axis',(0.,0.,-1.));
#11332=DIRECTION('center_axis',(1.,0.,0.));
#11333=DIRECTION('ref_axis',(0.,0.,-1.));
#11334=DIRECTION('axis',(0.,0.,1.));
#11335=DIRECTION('refdir',(1.,0.,0.));
#11336=DIRECTION('center_axis',(0.,0.,1.));
#11337=DIRECTION('ref_axis',(1.,0.,0.));
#11338=DIRECTION('center_axis',(0.,0.,-1.));
#11339=DIRECTION('ref_axis',(1.,0.,0.));
#11340=DIRECTION('',(0.,0.,-1.));
#11341=DIRECTION('center_axis',(0.,0.,-1.));
#11342=DIRECTION('ref_axis',(1.,0.,0.));
#11343=DIRECTION('center_axis',(0.,0.,1.));
#11344=DIRECTION('ref_axis',(1.,0.,0.));
#11345=DIRECTION('center_axis',(0.,0.,1.));
#11346=DIRECTION('ref_axis',(1.,0.,0.));
#11347=DIRECTION('',(0.,0.,-1.));
#11348=DIRECTION('center_axis',(0.,0.,1.));
#11349=DIRECTION('ref_axis',(1.,0.,0.));
#11350=DIRECTION('center_axis',(0.,0.,1.));
#11351=DIRECTION('ref_axis',(1.,0.,0.));
#11352=DIRECTION('center_axis',(0.,0.,1.));
#11353=DIRECTION('ref_axis',(1.,0.,0.));
#11354=DIRECTION('axis',(0.,0.,1.));
#11355=DIRECTION('refdir',(1.,0.,0.));
#11356=DIRECTION('axis',(0.,0.,1.));
#11357=DIRECTION('refdir',(1.,0.,0.));
#11358=DIRECTION('center_axis',(0.,0.,1.));
#11359=DIRECTION('ref_axis',(1.,0.,0.));
#11360=DIRECTION('',(-1.,0.,0.));
#11361=DIRECTION('center_axis',(0.,0.,1.));
#11362=DIRECTION('ref_axis',(1.,0.,0.));
#11363=DIRECTION('center_axis',(0.,0.,1.));
#11364=DIRECTION('ref_axis',(1.,0.,0.));
#11365=DIRECTION('',(0.,0.,-1.));
#11366=DIRECTION('center_axis',(0.,0.,1.));
#11367=DIRECTION('ref_axis',(1.,0.,0.));
#11368=DIRECTION('',(0.,0.,1.));
#11369=DIRECTION('center_axis',(0.,0.,-1.));
#11370=DIRECTION('ref_axis',(1.,0.,0.));
#11371=DIRECTION('center_axis',(0.,0.,1.));
#11372=DIRECTION('ref_axis',(1.,0.,0.));
#11373=DIRECTION('',(0.,0.,1.));
#11374=DIRECTION('center_axis',(0.,0.,1.));
#11375=DIRECTION('ref_axis',(1.,0.,0.));
#11376=DIRECTION('',(1.,0.,0.));
#11377=DIRECTION('center_axis',(0.,0.,1.));
#11378=DIRECTION('ref_axis',(1.,0.,0.));
#11379=DIRECTION('center_axis',(0.,0.,1.));
#11380=DIRECTION('ref_axis',(1.,0.,0.));
#11381=DIRECTION('',(0.,0.,-1.));
#11382=DIRECTION('center_axis',(0.,0.,1.));
#11383=DIRECTION('ref_axis',(1.,0.,0.));
#11384=DIRECTION('',(0.,0.,1.));
#11385=DIRECTION('center_axis',(0.,0.,-1.));
#11386=DIRECTION('ref_axis',(1.,0.,0.));
#11387=DIRECTION('center_axis',(0.,0.,1.));
#11388=DIRECTION('ref_axis',(1.,0.,0.));
#11389=DIRECTION('',(0.,0.,1.));
#11390=DIRECTION('center_axis',(0.,0.,1.));
#11391=DIRECTION('ref_axis',(1.,0.,0.));
#11392=DIRECTION('',(-1.,0.,0.));
#11393=DIRECTION('center_axis',(0.,0.,1.));
#11394=DIRECTION('ref_axis',(1.,0.,0.));
#11395=DIRECTION('center_axis',(0.,0.,1.));
#11396=DIRECTION('ref_axis',(1.,0.,0.));
#11397=DIRECTION('',(0.,0.,-1.));
#11398=DIRECTION('center_axis',(0.,0.,1.));
#11399=DIRECTION('ref_axis',(1.,0.,0.));
#11400=DIRECTION('',(0.,0.,1.));
#11401=DIRECTION('center_axis',(0.,0.,-1.));
#11402=DIRECTION('ref_axis',(1.,0.,0.));
#11403=DIRECTION('center_axis',(0.,0.,1.));
#11404=DIRECTION('ref_axis',(1.,0.,0.));
#11405=DIRECTION('',(0.,0.,1.));
#11406=DIRECTION('center_axis',(0.,0.,1.));
#11407=DIRECTION('ref_axis',(1.,0.,0.));
#11408=DIRECTION('',(1.,0.,0.));
#11409=DIRECTION('center_axis',(0.,0.,1.));
#11410=DIRECTION('ref_axis',(1.,0.,0.));
#11411=DIRECTION('center_axis',(0.,0.,1.));
#11412=DIRECTION('ref_axis',(1.,0.,0.));
#11413=DIRECTION('',(0.,0.,-1.));
#11414=DIRECTION('center_axis',(0.,0.,1.));
#11415=DIRECTION('ref_axis',(1.,0.,0.));
#11416=DIRECTION('',(0.,0.,1.));
#11417=DIRECTION('center_axis',(0.,0.,-1.));
#11418=DIRECTION('ref_axis',(1.,0.,0.));
#11419=DIRECTION('center_axis',(0.,0.,1.));
#11420=DIRECTION('ref_axis',(1.,0.,0.));
#11421=DIRECTION('',(0.,0.,1.));
#11422=DIRECTION('center_axis',(0.,-1.,0.));
#11423=DIRECTION('ref_axis',(0.,0.,-1.));
#11424=DIRECTION('',(-1.,0.,0.));
#11425=DIRECTION('',(-1.,0.,0.));
#11426=DIRECTION('',(0.,0.,1.));
#11427=DIRECTION('',(1.,0.,0.));
#11428=DIRECTION('',(0.,0.,-1.));
#11429=DIRECTION('',(-1.,0.,0.));
#11430=DIRECTION('center_axis',(0.,1.,0.));
#11431=DIRECTION('ref_axis',(0.,0.,1.));
#11432=DIRECTION('',(1.,0.,0.));
#11433=DIRECTION('',(1.,0.,0.));
#11434=DIRECTION('',(0.,0.,1.));
#11435=DIRECTION('',(1.,0.,0.));
#11436=DIRECTION('',(0.,0.,-1.));
#11437=DIRECTION('',(1.,0.,0.));
#11438=DIRECTION('center_axis',(-1.,0.,0.));
#11439=DIRECTION('ref_axis',(0.,0.,1.));
#11440=DIRECTION('',(0.,-1.,0.));
#11441=DIRECTION('',(0.,0.,1.));
#11442=DIRECTION('',(0.,1.,0.));
#11443=DIRECTION('',(0.,0.,-1.));
#11444=DIRECTION('',(0.,-1.,0.));
#11445=DIRECTION('',(0.,-1.,0.));
#11446=DIRECTION('',(0.,0.,1.));
#11447=DIRECTION('',(0.,-1.,0.));
#11448=DIRECTION('',(0.,0.,-1.));
#11449=DIRECTION('',(0.,-1.,0.));
#11450=DIRECTION('center_axis',(0.,0.,-1.));
#11451=DIRECTION('ref_axis',(0.,1.,0.));
#11452=DIRECTION('',(0.,1.,0.));
#11453=DIRECTION('',(1.,0.,0.));
#11454=DIRECTION('center_axis',(0.,-1.,0.));
#11455=DIRECTION('ref_axis',(0.,0.,-1.));
#11456=DIRECTION('',(0.,0.,-1.));
#11457=DIRECTION('',(1.,0.,0.));
#11458=DIRECTION('center_axis',(0.,0.,1.));
#11459=DIRECTION('ref_axis',(0.,-1.,0.));
#11460=DIRECTION('',(0.,-1.,0.));
#11461=DIRECTION('',(1.,0.,0.));
#11462=DIRECTION('center_axis',(0.,1.,0.));
#11463=DIRECTION('ref_axis',(0.,0.,1.));
#11464=DIRECTION('',(0.,0.,1.));
#11465=DIRECTION('',(1.,0.,0.));
#11466=DIRECTION('center_axis',(0.,0.,-1.));
#11467=DIRECTION('ref_axis',(0.,1.,0.));
#11468=DIRECTION('',(0.,1.,0.));
#11469=DIRECTION('center_axis',(0.,0.,-1.));
#11470=DIRECTION('ref_axis',(0.,1.,0.));
#11471=DIRECTION('',(0.,1.,0.));
#11472=DIRECTION('',(1.,0.,0.));
#11473=DIRECTION('center_axis',(0.,-1.,0.));
#11474=DIRECTION('ref_axis',(0.,0.,-1.));
#11475=DIRECTION('',(0.,0.,-1.));
#11476=DIRECTION('',(1.,0.,0.));
#11477=DIRECTION('center_axis',(0.,0.,-1.));
#11478=DIRECTION('ref_axis',(0.,1.,0.));
#11479=DIRECTION('',(0.,1.,0.));
#11480=DIRECTION('',(1.,0.,0.));
#11481=DIRECTION('center_axis',(0.,1.,0.));
#11482=DIRECTION('ref_axis',(0.,0.,1.));
#11483=DIRECTION('',(0.,0.,1.));
#11484=DIRECTION('',(1.,0.,0.));
#11485=DIRECTION('center_axis',(0.,0.,-1.));
#11486=DIRECTION('ref_axis',(0.,1.,0.));
#11487=DIRECTION('',(0.,1.,0.));
#11488=DIRECTION('center_axis',(1.,0.,0.));
#11489=DIRECTION('ref_axis',(0.,0.,-1.));
#11490=DIRECTION('axis',(0.,0.,1.));
#11491=DIRECTION('refdir',(1.,0.,0.));
#11492=DIRECTION('center_axis',(0.,0.,1.));
#11493=DIRECTION('ref_axis',(0.,-1.,0.));
#11494=DIRECTION('',(0.,-1.,0.));
#11495=DIRECTION('',(1.,0.,0.));
#11496=DIRECTION('',(0.,-1.,0.));
#11497=DIRECTION('',(1.,0.,0.));
#11498=DIRECTION('center_axis',(0.,1.,0.));
#11499=DIRECTION('ref_axis',(0.,0.,1.));
#11500=DIRECTION('',(0.,0.,1.));
#11501=DIRECTION('',(0.,0.,1.));
#11502=DIRECTION('',(1.,0.,0.));
#11503=DIRECTION('center_axis',(0.,0.,-1.));
#11504=DIRECTION('ref_axis',(0.,1.,0.));
#11505=DIRECTION('',(0.,1.,0.));
#11506=DIRECTION('',(0.,1.,0.));
#11507=DIRECTION('',(1.,0.,0.));
#11508=DIRECTION('center_axis',(0.,-1.,0.));
#11509=DIRECTION('ref_axis',(0.,0.,-1.));
#11510=DIRECTION('',(0.,0.,-1.));
#11511=DIRECTION('',(0.,0.,-1.));
#11512=DIRECTION('',(1.,0.,0.));
#11513=DIRECTION('center_axis',(0.,0.,-1.));
#11514=DIRECTION('ref_axis',(0.,1.,0.));
#11515=DIRECTION('',(0.,1.,0.));
#11516=DIRECTION('',(0.,1.,0.));
#11517=DIRECTION('',(1.,0.,0.));
#11518=DIRECTION('center_axis',(0.,1.,0.));
#11519=DIRECTION('ref_axis',(0.,0.,1.));
#11520=DIRECTION('',(0.,0.,1.));
#11521=DIRECTION('',(0.,0.,1.));
#11522=DIRECTION('',(1.,0.,0.));
#11523=DIRECTION('center_axis',(0.,0.,-1.));
#11524=DIRECTION('ref_axis',(0.,1.,0.));
#11525=DIRECTION('',(0.,1.,0.));
#11526=DIRECTION('',(0.,1.,0.));
#11527=DIRECTION('',(1.,0.,0.));
#11528=DIRECTION('center_axis',(0.,-1.,0.));
#11529=DIRECTION('ref_axis',(0.,0.,-1.));
#11530=DIRECTION('',(0.,0.,-1.));
#11531=DIRECTION('',(0.,0.,-1.));
#11532=DIRECTION('center_axis',(1.,0.,0.));
#11533=DIRECTION('ref_axis',(0.,0.,-1.));
#11534=DIRECTION('center_axis',(1.,0.,0.));
#11535=DIRECTION('ref_axis',(0.,0.,-1.));
#11536=DIRECTION('axis',(0.,0.,1.));
#11537=DIRECTION('refdir',(1.,0.,0.));
#11538=DIRECTION('center_axis',(0.,0.,-1.));
#11539=DIRECTION('ref_axis',(0.,-1.,0.));
#11540=DIRECTION('',(0.,1.,0.));
#11541=DIRECTION('',(-1.,0.,0.));
#11542=DIRECTION('',(0.,-1.,0.));
#11543=DIRECTION('',(-1.,0.,0.));
#11544=DIRECTION('center_axis',(0.,1.,0.));
#11545=DIRECTION('ref_axis',(0.,0.,-1.));
#11546=DIRECTION('',(0.,0.,1.));
#11547=DIRECTION('',(0.,0.,-1.));
#11548=DIRECTION('',(-1.,0.,0.));
#11549=DIRECTION('center_axis',(0.,0.,-1.));
#11550=DIRECTION('ref_axis',(0.,-1.,0.));
#11551=DIRECTION('',(0.,1.,0.));
#11552=DIRECTION('',(0.,-1.,0.));
#11553=DIRECTION('',(-1.,0.,0.));
#11554=DIRECTION('center_axis',(0.,-1.,0.));
#11555=DIRECTION('ref_axis',(0.,0.,1.));
#11556=DIRECTION('',(0.,0.,-1.));
#11557=DIRECTION('',(0.,0.,1.));
#11558=DIRECTION('',(-1.,0.,0.));
#11559=DIRECTION('center_axis',(0.,0.,-1.));
#11560=DIRECTION('ref_axis',(0.,-1.,0.));
#11561=DIRECTION('',(0.,1.,0.));
#11562=DIRECTION('',(0.,-1.,0.));
#11563=DIRECTION('',(-1.,0.,0.));
#11564=DIRECTION('center_axis',(0.,1.,0.));
#11565=DIRECTION('ref_axis',(0.,0.,-1.));
#11566=DIRECTION('',(0.,0.,1.));
#11567=DIRECTION('',(0.,0.,-1.));
#11568=DIRECTION('',(-1.,0.,0.));
#11569=DIRECTION('center_axis',(0.,0.,1.));
#11570=DIRECTION('ref_axis',(0.,1.,0.));
#11571=DIRECTION('',(0.,-1.,0.));
#11572=DIRECTION('',(0.,1.,0.));
#11573=DIRECTION('',(-1.,0.,0.));
#11574=DIRECTION('center_axis',(0.,-1.,0.));
#11575=DIRECTION('ref_axis',(0.,0.,1.));
#11576=DIRECTION('',(0.,0.,-1.));
#11577=DIRECTION('',(0.,0.,1.));
#11578=DIRECTION('center_axis',(1.,0.,0.));
#11579=DIRECTION('ref_axis',(0.,0.,-1.));
#11580=DIRECTION('center_axis',(-1.,0.,0.));
#11581=DIRECTION('ref_axis',(0.,0.,1.));
#11582=DIRECTION('',(0.,0.,1.));
#11583=DIRECTION('',(1.,0.,0.));
#11584=DIRECTION('',(0.,0.,1.));
#11585=DIRECTION('',(1.,0.,0.));
#11586=DIRECTION('',(0.,0.,1.));
#11587=DIRECTION('',(1.,0.,0.));
#11588=DIRECTION('axis',(0.,0.,1.));
#11589=DIRECTION('refdir',(1.,0.,0.));
#11590=DIRECTION('center_axis',(0.,1.,0.));
#11591=DIRECTION('ref_axis',(1.,0.,0.));
#11592=DIRECTION('center_axis',(0.,1.,0.));
#11593=DIRECTION('ref_axis',(1.,0.,0.));
#11594=DIRECTION('',(0.707106781186548,-0.707106781186547,-8.65956056235494E-17));
#11595=DIRECTION('center_axis',(0.,-1.,0.));
#11596=DIRECTION('ref_axis',(1.,0.,0.));
#11597=DIRECTION('center_axis',(0.,1.,0.));
#11598=DIRECTION('ref_axis',(1.,0.,0.));
#11599=DIRECTION('',(0.,-1.,0.));
#11600=DIRECTION('center_axis',(0.,-1.,0.));
#11601=DIRECTION('ref_axis',(1.,0.,0.));
#11602=DIRECTION('center_axis',(0.,1.,0.));
#11603=DIRECTION('ref_axis',(1.,0.,0.));
#11604=DIRECTION('center_axis',(0.,1.,0.));
#11605=DIRECTION('ref_axis',(1.,0.,0.));
#11606=DIRECTION('center_axis',(0.,1.,0.));
#11607=DIRECTION('ref_axis',(1.,0.,0.));
#11608=DIRECTION('',(0.,-1.,0.));
#11609=DIRECTION('center_axis',(0.,1.,0.));
#11610=DIRECTION('ref_axis',(1.,0.,0.));
#11611=DIRECTION('center_axis',(0.,1.,0.));
#11612=DIRECTION('ref_axis',(1.,0.,0.));
#11613=DIRECTION('axis',(0.,0.,1.));
#11614=DIRECTION('refdir',(1.,0.,0.));
#11615=DIRECTION('center_axis',(0.,1.,0.));
#11616=DIRECTION('ref_axis',(0.,0.,1.));
#11617=DIRECTION('center_axis',(0.,-1.,0.));
#11618=DIRECTION('ref_axis',(1.,0.,0.));
#11619=DIRECTION('center_axis',(0.,-1.,0.));
#11620=DIRECTION('ref_axis',(1.,0.,0.));
#11621=DIRECTION('center_axis',(0.,-1.,0.));
#11622=DIRECTION('ref_axis',(1.,0.,0.));
#11623=DIRECTION('',(0.707106781186548,0.707106781186547,8.65956056235493E-17));
#11624=DIRECTION('center_axis',(0.,-1.,0.));
#11625=DIRECTION('ref_axis',(1.,0.,0.));
#11626=DIRECTION('center_axis',(0.,-1.,0.));
#11627=DIRECTION('ref_axis',(1.,0.,0.));
#11628=DIRECTION('',(0.,1.,0.));
#11629=DIRECTION('center_axis',(0.,1.,0.));
#11630=DIRECTION('ref_axis',(1.,0.,0.));
#11631=DIRECTION('center_axis',(0.,-1.,0.));
#11632=DIRECTION('ref_axis',(1.,0.,0.));
#11633=DIRECTION('',(-0.707106781186547,0.707106781186548,-8.65956056235493E-17));
#11634=DIRECTION('center_axis',(0.,-1.,0.));
#11635=DIRECTION('ref_axis',(0.,0.,-1.));
#11636=DIRECTION('center_axis',(0.,-1.,0.));
#11637=DIRECTION('ref_axis',(1.,0.,0.));
#11638=DIRECTION('center_axis',(0.,1.,0.));
#11639=DIRECTION('ref_axis',(1.,0.,0.));
#11640=DIRECTION('center_axis',(0.,1.,0.));
#11641=DIRECTION('ref_axis',(1.,0.,0.));
#11642=DIRECTION('',(-0.447213595499958,0.894427190999916,-5.47678698264203E-17));
#11643=DIRECTION('center_axis',(0.,-1.,0.));
#11644=DIRECTION('ref_axis',(1.,0.,0.));
#11645=DIRECTION('center_axis',(0.,1.,0.));
#11646=DIRECTION('ref_axis',(1.,0.,0.));
#11647=DIRECTION('',(0.,1.,0.));
#11648=DIRECTION('center_axis',(0.,1.,0.));
#11649=DIRECTION('ref_axis',(1.,0.,0.));
#11650=DIRECTION('center_axis',(0.,-1.,0.));
#11651=DIRECTION('ref_axis',(1.,0.,0.));
#11652=DIRECTION('',(-0.707106781186547,0.707106781186548,-8.65956056235493E-17));
#11653=DIRECTION('center_axis',(0.,-1.,0.));
#11654=DIRECTION('ref_axis',(0.,0.,-1.));
#11655=DIRECTION('center_axis',(0.866025403784439,0.,-0.5));
#11656=DIRECTION('ref_axis',(0.5,0.,0.866025403784439));
#11657=DIRECTION('',(-0.5,0.,-0.866025403784439));
#11658=DIRECTION('',(0.,-1.,0.));
#11659=DIRECTION('',(0.5,0.,0.866025403784439));
#11660=DIRECTION('',(0.,-1.,0.));
#11661=DIRECTION('center_axis',(1.20185167898973E-16,0.,-1.));
#11662=DIRECTION('ref_axis',(1.,0.,1.20185167898973E-16));
#11663=DIRECTION('',(-1.,0.,-1.20185167898973E-16));
#11664=DIRECTION('',(0.,-1.,0.));
#11665=DIRECTION('',(1.,0.,1.20185167898973E-16));
#11666=DIRECTION('center_axis',(-0.866025403784439,0.,-0.5));
#11667=DIRECTION('ref_axis',(0.5,0.,-0.866025403784439));
#11668=DIRECTION('',(-0.5,0.,0.866025403784439));
#11669=DIRECTION('',(0.,-1.,0.));
#11670=DIRECTION('',(0.5,0.,-0.866025403784439));
#11671=DIRECTION('center_axis',(-0.866025403784439,0.,0.5));
#11672=DIRECTION('ref_axis',(-0.5,0.,-0.866025403784439));
#11673=DIRECTION('',(0.5,0.,0.866025403784439));
#11674=DIRECTION('',(0.,-1.,0.));
#11675=DIRECTION('',(-0.5,0.,-0.866025403784439));
#11676=DIRECTION('center_axis',(-2.40370335797945E-16,0.,1.));
#11677=DIRECTION('ref_axis',(-1.,0.,-2.40370335797945E-16));
#11678=DIRECTION('',(1.,0.,2.40370335797945E-16));
#11679=DIRECTION('',(0.,-1.,0.));
#11680=DIRECTION('',(-1.,0.,-2.40370335797945E-16));
#11681=DIRECTION('center_axis',(0.866025403784439,0.,0.5));
#11682=DIRECTION('ref_axis',(-0.5,0.,0.866025403784439));
#11683=DIRECTION('',(0.5,0.,-0.866025403784439));
#11684=DIRECTION('',(-0.5,0.,0.866025403784439));
#11685=DIRECTION('center_axis',(0.,1.,0.));
#11686=DIRECTION('ref_axis',(1.,0.,0.));
#11687=DIRECTION('center_axis',(0.,-1.,0.));
#11688=DIRECTION('ref_axis',(0.,0.,-1.));
#11689=DIRECTION('axis',(0.,0.,1.));
#11690=DIRECTION('refdir',(1.,0.,0.));
#11691=DIRECTION('center_axis',(0.,1.,0.));
#11692=DIRECTION('ref_axis',(1.,0.,0.));
#11693=DIRECTION('center_axis',(0.,1.,0.));
#11694=DIRECTION('ref_axis',(1.,0.,0.));
#11695=DIRECTION('',(0.707106781186547,-0.707106781186548,-8.65956056235493E-17));
#11696=DIRECTION('center_axis',(0.,-1.,0.));
#11697=DIRECTION('ref_axis',(1.,0.,0.));
#11698=DIRECTION('center_axis',(0.,1.,0.));
#11699=DIRECTION('ref_axis',(1.,0.,0.));
#11700=DIRECTION('',(0.,-1.,0.));
#11701=DIRECTION('center_axis',(0.,-1.,0.));
#11702=DIRECTION('ref_axis',(1.,0.,0.));
#11703=DIRECTION('center_axis',(0.,1.,0.));
#11704=DIRECTION('ref_axis',(1.,0.,0.));
#11705=DIRECTION('center_axis',(0.,1.,0.));
#11706=DIRECTION('ref_axis',(1.,0.,0.));
#11707=DIRECTION('center_axis',(0.,1.,0.));
#11708=DIRECTION('ref_axis',(1.,0.,0.));
#11709=DIRECTION('',(0.,-1.,0.));
#11710=DIRECTION('center_axis',(0.,1.,0.));
#11711=DIRECTION('ref_axis',(1.,0.,0.));
#11712=DIRECTION('center_axis',(0.,1.,0.));
#11713=DIRECTION('ref_axis',(1.,0.,0.));
#11714=DIRECTION('axis',(0.,0.,1.));
#11715=DIRECTION('refdir',(1.,0.,0.));
#11716=DIRECTION('center_axis',(0.,1.,0.));
#11717=DIRECTION('ref_axis',(0.,0.,1.));
#11718=DIRECTION('center_axis',(0.,-1.,0.));
#11719=DIRECTION('ref_axis',(1.,0.,0.));
#11720=DIRECTION('center_axis',(0.,-1.,0.));
#11721=DIRECTION('ref_axis',(1.,0.,0.));
#11722=DIRECTION('center_axis',(0.,-1.,0.));
#11723=DIRECTION('ref_axis',(1.,0.,0.));
#11724=DIRECTION('',(0.707106781186547,0.707106781186548,8.65956056235493E-17));
#11725=DIRECTION('center_axis',(0.,-1.,0.));
#11726=DIRECTION('ref_axis',(1.,0.,0.));
#11727=DIRECTION('center_axis',(0.,-1.,0.));
#11728=DIRECTION('ref_axis',(1.,0.,0.));
#11729=DIRECTION('',(0.,1.,0.));
#11730=DIRECTION('center_axis',(0.,1.,0.));
#11731=DIRECTION('ref_axis',(1.,0.,0.));
#11732=DIRECTION('center_axis',(0.,-1.,0.));
#11733=DIRECTION('ref_axis',(1.,0.,0.));
#11734=DIRECTION('',(-0.707106781186547,0.707106781186548,-8.65956056235493E-17));
#11735=DIRECTION('center_axis',(0.,-1.,0.));
#11736=DIRECTION('ref_axis',(0.,0.,-1.));
#11737=DIRECTION('center_axis',(0.,-1.,0.));
#11738=DIRECTION('ref_axis',(1.,0.,0.));
#11739=DIRECTION('center_axis',(0.,1.,0.));
#11740=DIRECTION('ref_axis',(1.,0.,0.));
#11741=DIRECTION('center_axis',(0.,1.,0.));
#11742=DIRECTION('ref_axis',(1.,0.,0.));
#11743=DIRECTION('',(-0.447213595499958,0.894427190999916,-5.47678698264203E-17));
#11744=DIRECTION('center_axis',(0.,-1.,0.));
#11745=DIRECTION('ref_axis',(1.,0.,0.));
#11746=DIRECTION('center_axis',(0.,1.,0.));
#11747=DIRECTION('ref_axis',(1.,0.,0.));
#11748=DIRECTION('',(0.,1.,0.));
#11749=DIRECTION('center_axis',(0.,1.,0.));
#11750=DIRECTION('ref_axis',(1.,0.,0.));
#11751=DIRECTION('center_axis',(0.,-1.,0.));
#11752=DIRECTION('ref_axis',(1.,0.,0.));
#11753=DIRECTION('',(-0.707106781186547,0.707106781186548,-8.65956056235493E-17));
#11754=DIRECTION('center_axis',(0.,-1.,0.));
#11755=DIRECTION('ref_axis',(0.,0.,-1.));
#11756=DIRECTION('center_axis',(0.866025403784439,0.,-0.5));
#11757=DIRECTION('ref_axis',(0.5,0.,0.866025403784439));
#11758=DIRECTION('',(-0.5,0.,-0.866025403784439));
#11759=DIRECTION('',(0.,-1.,0.));
#11760=DIRECTION('',(0.5,0.,0.866025403784439));
#11761=DIRECTION('',(0.,-1.,0.));
#11762=DIRECTION('center_axis',(1.60246890531964E-16,0.,-1.));
#11763=DIRECTION('ref_axis',(1.,0.,1.60246890531964E-16));
#11764=DIRECTION('',(-1.,0.,-1.60246890531964E-16));
#11765=DIRECTION('',(0.,-1.,0.));
#11766=DIRECTION('',(1.,0.,1.60246890531964E-16));
#11767=DIRECTION('center_axis',(-0.866025403784439,0.,-0.5));
#11768=DIRECTION('ref_axis',(0.5,0.,-0.866025403784439));
#11769=DIRECTION('',(-0.5,0.,0.866025403784439));
#11770=DIRECTION('',(0.,-1.,0.));
#11771=DIRECTION('',(0.5,0.,-0.866025403784439));
#11772=DIRECTION('center_axis',(-0.866025403784439,0.,0.5));
#11773=DIRECTION('ref_axis',(-0.5,0.,-0.866025403784439));
#11774=DIRECTION('',(0.5,0.,0.866025403784439));
#11775=DIRECTION('',(0.,-1.,0.));
#11776=DIRECTION('',(-0.5,0.,-0.866025403784439));
#11777=DIRECTION('center_axis',(-1.60246890531964E-16,0.,1.));
#11778=DIRECTION('ref_axis',(-1.,0.,-1.60246890531964E-16));
#11779=DIRECTION('',(1.,0.,1.60246890531964E-16));
#11780=DIRECTION('',(0.,-1.,0.));
#11781=DIRECTION('',(-1.,0.,-1.60246890531964E-16));
#11782=DIRECTION('center_axis',(0.866025403784439,0.,0.5));
#11783=DIRECTION('ref_axis',(-0.5,0.,0.866025403784439));
#11784=DIRECTION('',(0.5,0.,-0.866025403784439));
#11785=DIRECTION('',(-0.5,0.,0.866025403784439));
#11786=DIRECTION('center_axis',(0.,1.,0.));
#11787=DIRECTION('ref_axis',(1.,0.,0.));
#11788=DIRECTION('center_axis',(0.,-1.,0.));
#11789=DIRECTION('ref_axis',(0.,0.,-1.));
#11790=DIRECTION('',(0.,0.,1.));
#11791=DIRECTION('',(1.,0.,0.));
#11792=DIRECTION('',(0.,0.,1.));
#11793=DIRECTION('',(1.,0.,0.));
#11794=DIRECTION('',(0.,0.,1.));
#11795=DIRECTION('',(1.,0.,0.));
#11796=DIRECTION('',(0.,0.,1.));
#11797=DIRECTION('',(1.,0.,0.));
#11798=DIRECTION('',(0.,0.,1.));
#11799=DIRECTION('',(1.,0.,0.));
#11800=DIRECTION('',(0.,0.,1.));
#11801=DIRECTION('',(1.,0.,0.));
#11802=DIRECTION('',(0.,0.,1.));
#11803=DIRECTION('',(1.,0.,0.));
#11804=DIRECTION('',(0.,0.,1.));
#11805=DIRECTION('',(1.,0.,0.));
#11806=DIRECTION('',(0.,0.,1.));
#11807=DIRECTION('',(1.,0.,0.));
#11808=DIRECTION('',(0.,0.,1.));
#11809=DIRECTION('',(1.,0.,0.));
#11810=DIRECTION('',(0.,0.,1.));
#11811=DIRECTION('',(1.,0.,0.));
#11812=DIRECTION('',(0.,0.,1.));
#11813=DIRECTION('',(1.,0.,0.));
#11814=DIRECTION('',(0.,0.,1.));
#11815=DIRECTION('',(1.,0.,0.));
#11816=DIRECTION('',(0.,0.,1.));
#11817=DIRECTION('',(1.,0.,0.));
#11818=DIRECTION('',(0.,-1.,2.22044604925031E-16));
#11819=DIRECTION('',(1.,0.,0.));
#11820=DIRECTION('',(0.,-1.,2.22044604925031E-16));
#11821=DIRECTION('',(1.,0.,0.));
#11822=DIRECTION('',(0.,0.,1.));
#11823=DIRECTION('',(1.,0.,0.));
#11824=DIRECTION('',(0.,-1.,2.22044604925031E-16));
#11825=DIRECTION('',(1.,0.,0.));
#11826=DIRECTION('',(0.,-1.,2.22044604925031E-16));
#11827=DIRECTION('',(1.,0.,0.));
#11828=DIRECTION('',(0.,0.,1.));
#11829=DIRECTION('',(1.,0.,0.));
#11830=DIRECTION('',(0.,-1.,2.22044604925031E-16));
#11831=DIRECTION('',(1.,0.,0.));
#11832=DIRECTION('',(0.,-1.,2.22044604925031E-16));
#11833=DIRECTION('',(1.,0.,0.));
#11834=DIRECTION('',(0.,0.,1.));
#11835=DIRECTION('',(1.,0.,0.));
#11836=DIRECTION('',(0.,-1.,2.22044604925031E-16));
#11837=DIRECTION('',(1.,0.,0.));
#11838=DIRECTION('',(0.,-1.,2.22044604925031E-16));
#11839=DIRECTION('',(1.,0.,0.));
#11840=DIRECTION('',(0.,-1.,2.22044604925031E-16));
#11841=DIRECTION('',(1.,0.,0.));
#11842=DIRECTION('',(0.,-1.,2.22044604925031E-16));
#11843=DIRECTION('',(1.,0.,0.));
#11844=DIRECTION('',(0.,-1.,2.22044604925031E-16));
#11845=DIRECTION('',(1.,0.,0.));
#11846=DIRECTION('',(0.,-1.,2.22044604925031E-16));
#11847=DIRECTION('',(1.,0.,0.));
#11848=DIRECTION('',(0.,-1.,2.22044604925031E-16));
#11849=DIRECTION('',(1.,0.,0.));
#11850=DIRECTION('',(0.,-1.,2.22044604925031E-16));
#11851=DIRECTION('',(1.,0.,0.));
#11852=DIRECTION('',(0.,-1.,2.22044604925031E-16));
#11853=DIRECTION('',(1.,0.,0.));
#11854=DIRECTION('',(0.,-1.,2.22044604925031E-16));
#11855=DIRECTION('',(1.,0.,0.));
#11856=DIRECTION('',(0.,-1.,2.22044604925031E-16));
#11857=DIRECTION('',(1.,0.,0.));
#11858=DIRECTION('',(0.,-1.,2.22044604925031E-16));
#11859=DIRECTION('',(1.,0.,0.));
#11860=DIRECTION('',(0.,-1.,2.22044604925031E-16));
#11861=DIRECTION('',(1.,0.,0.));
#11862=DIRECTION('',(0.,-1.,2.22044604925031E-16));
#11863=DIRECTION('',(1.,0.,0.));
#11864=DIRECTION('axis',(0.,0.,1.));
#11865=DIRECTION('refdir',(1.,0.,0.));
#11866=DIRECTION('center_axis',(0.,1.,0.));
#11867=DIRECTION('ref_axis',(1.,0.,0.));
#11868=DIRECTION('center_axis',(0.,-1.,0.));
#11869=DIRECTION('ref_axis',(1.,0.,0.));
#11870=DIRECTION('',(0.,-1.,0.));
#11871=DIRECTION('center_axis',(0.,-1.,0.));
#11872=DIRECTION('ref_axis',(1.,0.,0.));
#11873=DIRECTION('center_axis',(0.,1.,0.));
#11874=DIRECTION('ref_axis',(1.,0.,0.));
#11875=DIRECTION('center_axis',(0.,1.,0.));
#11876=DIRECTION('ref_axis',(1.,0.,0.));
#11877=DIRECTION('',(0.,-1.,0.));
#11878=DIRECTION('center_axis',(0.,1.,0.));
#11879=DIRECTION('ref_axis',(1.,0.,0.));
#11880=DIRECTION('center_axis',(0.,1.,0.));
#11881=DIRECTION('ref_axis',(1.,0.,0.));
#11882=DIRECTION('center_axis',(0.,1.,0.));
#11883=DIRECTION('ref_axis',(1.,0.,0.));
#11884=DIRECTION('axis',(0.,0.,1.));
#11885=DIRECTION('refdir',(1.,0.,0.));
#11886=DIRECTION('center_axis',(0.,1.,0.));
#11887=DIRECTION('ref_axis',(0.,0.,1.));
#11888=DIRECTION('center_axis',(0.,-1.,0.));
#11889=DIRECTION('ref_axis',(1.,0.,0.));
#11890=DIRECTION('center_axis',(0.,-1.,0.));
#11891=DIRECTION('ref_axis',(1.,0.,0.));
#11892=DIRECTION('center_axis',(0.,-1.,0.));
#11893=DIRECTION('ref_axis',(1.,0.,0.));
#11894=DIRECTION('',(0.707106781186548,0.707106781186547,8.65956056235494E-17));
#11895=DIRECTION('center_axis',(0.,-1.,0.));
#11896=DIRECTION('ref_axis',(1.,0.,0.));
#11897=DIRECTION('center_axis',(0.,-1.,0.));
#11898=DIRECTION('ref_axis',(1.,0.,0.));
#11899=DIRECTION('',(0.,1.,0.));
#11900=DIRECTION('center_axis',(0.,1.,0.));
#11901=DIRECTION('ref_axis',(1.,0.,0.));
#11902=DIRECTION('center_axis',(0.,-1.,0.));
#11903=DIRECTION('ref_axis',(1.,0.,0.));
#11904=DIRECTION('',(-0.707106781186547,0.707106781186548,-8.65956056235493E-17));
#11905=DIRECTION('center_axis',(0.,-1.,0.));
#11906=DIRECTION('ref_axis',(0.,0.,-1.));
#11907=DIRECTION('center_axis',(0.,-1.,0.));
#11908=DIRECTION('ref_axis',(1.,0.,0.));
#11909=DIRECTION('center_axis',(0.,1.,0.));
#11910=DIRECTION('ref_axis',(1.,0.,0.));
#11911=DIRECTION('center_axis',(0.,1.,0.));
#11912=DIRECTION('ref_axis',(1.,0.,0.));
#11913=DIRECTION('',(-0.447213595499958,0.894427190999916,-5.47678698264203E-17));
#11914=DIRECTION('center_axis',(0.,-1.,0.));
#11915=DIRECTION('ref_axis',(1.,0.,0.));
#11916=DIRECTION('center_axis',(0.,1.,0.));
#11917=DIRECTION('ref_axis',(1.,0.,0.));
#11918=DIRECTION('',(0.,1.,0.));
#11919=DIRECTION('center_axis',(0.,1.,0.));
#11920=DIRECTION('ref_axis',(1.,0.,0.));
#11921=DIRECTION('center_axis',(0.,-1.,0.));
#11922=DIRECTION('ref_axis',(1.,0.,0.));
#11923=DIRECTION('',(-0.707106781186547,0.707106781186548,-8.65956056235493E-17));
#11924=DIRECTION('center_axis',(0.,-1.,0.));
#11925=DIRECTION('ref_axis',(0.,0.,-1.));
#11926=DIRECTION('center_axis',(0.866025403784439,0.,-0.5));
#11927=DIRECTION('ref_axis',(0.5,0.,0.866025403784439));
#11928=DIRECTION('',(-0.5,0.,-0.866025403784439));
#11929=DIRECTION('',(0.,-1.,0.));
#11930=DIRECTION('',(0.5,0.,0.866025403784439));
#11931=DIRECTION('',(0.,-1.,0.));
#11932=DIRECTION('center_axis',(1.92296268638356E-16,0.,-1.));
#11933=DIRECTION('ref_axis',(1.,0.,1.92296268638356E-16));
#11934=DIRECTION('',(-1.,0.,-1.92296268638356E-16));
#11935=DIRECTION('',(0.,-1.,0.));
#11936=DIRECTION('',(1.,0.,1.92296268638356E-16));
#11937=DIRECTION('center_axis',(-0.866025403784439,0.,-0.5));
#11938=DIRECTION('ref_axis',(0.5,0.,-0.866025403784439));
#11939=DIRECTION('',(-0.5,0.,0.866025403784438));
#11940=DIRECTION('',(0.,-1.,0.));
#11941=DIRECTION('',(0.5,0.,-0.866025403784438));
#11942=DIRECTION('center_axis',(-0.866025403784439,0.,0.5));
#11943=DIRECTION('ref_axis',(-0.5,0.,-0.866025403784439));
#11944=DIRECTION('',(0.5,0.,0.866025403784439));
#11945=DIRECTION('',(0.,-1.,0.));
#11946=DIRECTION('',(-0.5,0.,-0.866025403784439));
#11947=DIRECTION('center_axis',(-1.92296268638356E-16,0.,1.));
#11948=DIRECTION('ref_axis',(-1.,0.,-1.92296268638356E-16));
#11949=DIRECTION('',(1.,0.,1.92296268638356E-16));
#11950=DIRECTION('',(0.,-1.,0.));
#11951=DIRECTION('',(-1.,0.,-1.92296268638356E-16));
#11952=DIRECTION('center_axis',(0.866025403784439,0.,0.5));
#11953=DIRECTION('ref_axis',(-0.5,0.,0.866025403784439));
#11954=DIRECTION('',(0.5,0.,-0.866025403784439));
#11955=DIRECTION('',(-0.5,0.,0.866025403784439));
#11956=DIRECTION('center_axis',(0.,1.,0.));
#11957=DIRECTION('ref_axis',(1.,0.,0.));
#11958=DIRECTION('center_axis',(0.,-1.,0.));
#11959=DIRECTION('ref_axis',(0.,0.,-1.));
#11960=DIRECTION('',(0.,0.,1.));
#11961=DIRECTION('',(1.,0.,0.));
#11962=DIRECTION('',(0.,0.,1.));
#11963=DIRECTION('',(1.,0.,0.));
#11964=DIRECTION('',(0.,0.,1.));
#11965=DIRECTION('',(1.,0.,0.));
#11966=DIRECTION('',(0.,0.,1.));
#11967=DIRECTION('',(1.,0.,0.));
#11968=DIRECTION('',(0.,-1.,2.22044604925031E-16));
#11969=DIRECTION('',(1.,0.,0.));
#11970=DIRECTION('',(0.,-1.,2.22044604925031E-16));
#11971=DIRECTION('',(1.,0.,0.));
#11972=DIRECTION('',(0.,-1.,2.22044604925031E-16));
#11973=DIRECTION('',(1.,0.,0.));
#11974=DIRECTION('',(0.,-1.,2.22044604925031E-16));
#11975=DIRECTION('',(1.,0.,0.));
#11976=DIRECTION('',(0.,-1.,2.22044604925031E-16));
#11977=DIRECTION('',(1.,0.,0.));
#11978=DIRECTION('',(0.,-1.,2.22044604925031E-16));
#11979=DIRECTION('',(1.,0.,0.));
#11980=DIRECTION('',(0.,-1.,2.22044604925031E-16));
#11981=DIRECTION('',(1.,0.,0.));
#11982=DIRECTION('',(0.,-1.,2.22044604925031E-16));
#11983=DIRECTION('',(1.,0.,0.));
#11984=DIRECTION('',(0.,-1.,2.22044604925031E-16));
#11985=DIRECTION('',(1.,0.,0.));
#11986=DIRECTION('',(0.,-1.,2.22044604925031E-16));
#11987=DIRECTION('',(1.,0.,0.));
#11988=DIRECTION('',(0.,-1.,2.22044604925031E-16));
#11989=DIRECTION('',(1.,0.,0.));
#11990=DIRECTION('',(0.,-1.,2.22044604925031E-16));
#11991=DIRECTION('',(1.,0.,0.));
#11992=DIRECTION('',(0.,0.,1.));
#11993=DIRECTION('',(1.,0.,0.));
#11994=DIRECTION('',(0.,0.,1.));
#11995=DIRECTION('',(1.,0.,0.));
#11996=CARTESIAN_POINT('',(0.,0.,0.));
#11997=CARTESIAN_POINT('',(0.,0.,0.));
#11998=CARTESIAN_POINT('',(0.,0.,0.));
#11999=CARTESIAN_POINT('Origin',(2.,4.4,1.9));
#12000=CARTESIAN_POINT('',(1.835,4.4,2.));
#12001=CARTESIAN_POINT('Origin',(2.,4.4,2.));
#12002=CARTESIAN_POINT('',(1.835,4.4,2.8));
#12003=CARTESIAN_POINT('',(1.835,4.4,1.9));
#12004=CARTESIAN_POINT('Origin',(2.,4.4,2.8));
#12005=CARTESIAN_POINT('Origin',(20.,4.4,1.9));
#12006=CARTESIAN_POINT('',(19.835,4.4,2.));
#12007=CARTESIAN_POINT('Origin',(20.,4.4,2.));
#12008=CARTESIAN_POINT('',(19.835,4.4,2.8));
#12009=CARTESIAN_POINT('',(19.835,4.4,1.9));
#12010=CARTESIAN_POINT('Origin',(20.,4.4,2.8));
#12011=CARTESIAN_POINT('Origin',(23.,-2.4,1.9));
#12012=CARTESIAN_POINT('',(22.79,-2.4,2.));
#12013=CARTESIAN_POINT('Origin',(23.,-2.4,2.));
#12014=CARTESIAN_POINT('',(22.79,-2.4,2.8));
#12015=CARTESIAN_POINT('',(22.79,-2.4,1.9));
#12016=CARTESIAN_POINT('Origin',(23.,-2.4,2.8));
#12017=CARTESIAN_POINT('Origin',(-1.,2.4,1.9));
#12018=CARTESIAN_POINT('',(-1.21,2.4,2.));
#12019=CARTESIAN_POINT('Origin',(-1.,2.4,2.));
#12020=CARTESIAN_POINT('',(-1.21,2.4,2.8));
#12021=CARTESIAN_POINT('',(-1.21,2.4,1.9));
#12022=CARTESIAN_POINT('Origin',(-1.,2.4,2.8));
#12023=CARTESIAN_POINT('Origin',(-1.,-2.4,1.9));
#12024=CARTESIAN_POINT('',(-1.21,-2.4,2.));
#12025=CARTESIAN_POINT('Origin',(-1.,-2.4,2.));
#12026=CARTESIAN_POINT('',(-1.21,-2.4,2.8));
#12027=CARTESIAN_POINT('',(-1.21,-2.4,1.9));
#12028=CARTESIAN_POINT('Origin',(-1.,-2.4,2.8));
#12029=CARTESIAN_POINT('Origin',(23.,2.4,1.9));
#12030=CARTESIAN_POINT('',(22.79,2.4,2.));
#12031=CARTESIAN_POINT('Origin',(23.,2.4,2.));
#12032=CARTESIAN_POINT('',(22.79,2.4,2.8));
#12033=CARTESIAN_POINT('',(22.79,2.4,1.9));
#12034=CARTESIAN_POINT('Origin',(23.,2.4,2.8));
#12035=CARTESIAN_POINT('Origin',(19.5,-3.5,1.9));
#12036=CARTESIAN_POINT('',(19.225,-3.5,2.));
#12037=CARTESIAN_POINT('Origin',(19.5,-3.5,2.));
#12038=CARTESIAN_POINT('',(19.225,-3.5,2.8));
#12039=CARTESIAN_POINT('',(19.225,-3.5,1.9));
#12040=CARTESIAN_POINT('Origin',(19.5,-3.5,2.8));
#12041=CARTESIAN_POINT('Origin',(2.5,3.5,1.9));
#12042=CARTESIAN_POINT('',(2.225,3.5,2.));
#12043=CARTESIAN_POINT('Origin',(2.5,3.5,2.));
#12044=CARTESIAN_POINT('',(2.225,3.5,2.8));
#12045=CARTESIAN_POINT('',(2.225,3.5,1.9));
#12046=CARTESIAN_POINT('Origin',(2.5,3.5,2.8));
#12047=CARTESIAN_POINT('Origin',(2.5,-3.5,1.9));
#12048=CARTESIAN_POINT('',(2.225,-3.5,2.));
#12049=CARTESIAN_POINT('Origin',(2.5,-3.5,2.));
#12050=CARTESIAN_POINT('',(2.225,-3.5,2.8));
#12051=CARTESIAN_POINT('',(2.225,-3.5,1.9));
#12052=CARTESIAN_POINT('Origin',(2.5,-3.5,2.8));
#12053=CARTESIAN_POINT('Origin',(19.5,3.5,1.9));
#12054=CARTESIAN_POINT('',(19.225,3.5,2.));
#12055=CARTESIAN_POINT('Origin',(19.5,3.5,2.));
#12056=CARTESIAN_POINT('',(19.225,3.5,2.8));
#12057=CARTESIAN_POINT('',(19.225,3.5,1.9));
#12058=CARTESIAN_POINT('Origin',(19.5,3.5,2.8));
#12059=CARTESIAN_POINT('Origin',(14.,0.,1.9));
#12060=CARTESIAN_POINT('',(13.835,-2.02066721859312E-17,2.));
#12061=CARTESIAN_POINT('Origin',(14.,0.,2.));
#12062=CARTESIAN_POINT('',(13.835,2.02066721859312E-17,2.8));
#12063=CARTESIAN_POINT('',(13.835,-2.02066721859312E-17,1.9));
#12064=CARTESIAN_POINT('Origin',(14.,0.,2.8));
#12065=CARTESIAN_POINT('Origin',(8.,0.,1.9));
#12066=CARTESIAN_POINT('',(7.835,-2.02066721859312E-17,2.));
#12067=CARTESIAN_POINT('Origin',(8.,0.,2.));
#12068=CARTESIAN_POINT('',(7.835,2.02066721859312E-17,2.8));
#12069=CARTESIAN_POINT('',(7.835,-2.02066721859312E-17,1.9));
#12070=CARTESIAN_POINT('Origin',(8.,0.,2.8));
#12071=CARTESIAN_POINT('Origin',(2.,0.,1.9));
#12072=CARTESIAN_POINT('',(1.835,-2.02066721859313E-17,2.));
#12073=CARTESIAN_POINT('Origin',(2.,0.,2.));
#12074=CARTESIAN_POINT('',(1.835,2.02066721859313E-17,2.8));
#12075=CARTESIAN_POINT('',(1.835,-2.02066721859313E-17,1.9));
#12076=CARTESIAN_POINT('Origin',(2.,0.,2.8));
#12077=CARTESIAN_POINT('Origin',(20.,0.,1.9));
#12078=CARTESIAN_POINT('',(19.835,-2.02066721859312E-17,2.));
#12079=CARTESIAN_POINT('Origin',(20.,0.,2.));
#12080=CARTESIAN_POINT('',(19.835,2.02066721859312E-17,2.8));
#12081=CARTESIAN_POINT('',(19.835,-2.02066721859312E-17,1.9));
#12082=CARTESIAN_POINT('Origin',(20.,0.,2.8));
#12083=CARTESIAN_POINT('Origin',(24.,5.,2.));
#12084=CARTESIAN_POINT('',(24.,5.,2.));
#12085=CARTESIAN_POINT('',(-2.,5.,2.));
#12086=CARTESIAN_POINT('',(24.,5.,2.));
#12087=CARTESIAN_POINT('',(-2.,5.,2.8));
#12088=CARTESIAN_POINT('',(-2.,5.,2.));
#12089=CARTESIAN_POINT('',(24.,5.,2.8));
#12090=CARTESIAN_POINT('',(24.,5.,2.8));
#12091=CARTESIAN_POINT('',(24.,5.,2.));
#12092=CARTESIAN_POINT('Origin',(24.,-5.,2.));
#12093=CARTESIAN_POINT('',(24.,-5.,2.));
#12094=CARTESIAN_POINT('',(24.,-5.,2.));
#12095=CARTESIAN_POINT('',(24.,-5.,2.8));
#12096=CARTESIAN_POINT('',(24.,-5.,2.8));
#12097=CARTESIAN_POINT('',(24.,-5.,2.));
#12098=CARTESIAN_POINT('Origin',(-2.,-5.,2.));
#12099=CARTESIAN_POINT('',(-2.,-5.,2.));
#12100=CARTESIAN_POINT('',(-2.,-5.,2.));
#12101=CARTESIAN_POINT('',(-2.,-5.,2.8));
#12102=CARTESIAN_POINT('',(-2.,-5.,2.8));
#12103=CARTESIAN_POINT('',(-2.,-5.,2.));
#12104=CARTESIAN_POINT('Origin',(-2.,5.,2.));
#12105=CARTESIAN_POINT('',(-2.,5.,2.));
#12106=CARTESIAN_POINT('',(-2.,5.,2.8));
#12107=CARTESIAN_POINT('Origin',(11.,0.,2.8));
#12108=CARTESIAN_POINT('Origin',(11.,0.,2.));
#12109=CARTESIAN_POINT('',(0.,0.,0.));
#12110=CARTESIAN_POINT('Origin',(-1.,-2.4,4.));
#12111=CARTESIAN_POINT('',(-1.475,-2.4,4.));
#12112=CARTESIAN_POINT('Origin',(-1.,-2.4,4.));
#12113=CARTESIAN_POINT('',(-1.475,-2.4,6.2));
#12114=CARTESIAN_POINT('',(-1.475,-2.4,4.));
#12115=CARTESIAN_POINT('Origin',(-1.,-2.4,6.2));
#12116=CARTESIAN_POINT('Origin',(-1.,-2.4,4.));
#12117=CARTESIAN_POINT('',(-1.275,-2.4,4.));
#12118=CARTESIAN_POINT('Origin',(-1.,-2.4,4.));
#12119=CARTESIAN_POINT('Origin',(-1.,2.4,4.));
#12120=CARTESIAN_POINT('',(-1.475,2.4,4.));
#12121=CARTESIAN_POINT('Origin',(-1.,2.4,4.));
#12122=CARTESIAN_POINT('',(-1.475,2.4,6.2));
#12123=CARTESIAN_POINT('',(-1.475,2.4,4.));
#12124=CARTESIAN_POINT('Origin',(-1.,2.4,6.2));
#12125=CARTESIAN_POINT('Origin',(-1.,2.4,4.));
#12126=CARTESIAN_POINT('',(-1.275,2.4,4.));
#12127=CARTESIAN_POINT('Origin',(-1.,2.4,4.));
#12128=CARTESIAN_POINT('Origin',(-1.,-2.4,2.7));
#12129=CARTESIAN_POINT('',(-1.275,-2.4,2.8));
#12130=CARTESIAN_POINT('Origin',(-1.,-2.4,2.8));
#12131=CARTESIAN_POINT('',(-1.275,-2.4,2.7));
#12132=CARTESIAN_POINT('Origin',(-1.,2.4,2.7));
#12133=CARTESIAN_POINT('',(-1.275,2.4,2.8));
#12134=CARTESIAN_POINT('Origin',(-1.,2.4,2.8));
#12135=CARTESIAN_POINT('',(-1.275,2.4,2.7));
#12136=CARTESIAN_POINT('Origin',(0.,3.2,2.8));
#12137=CARTESIAN_POINT('',(0.,3.2,2.8));
#12138=CARTESIAN_POINT('',(-2.,3.2,2.8));
#12139=CARTESIAN_POINT('',(0.,3.2,2.8));
#12140=CARTESIAN_POINT('',(-2.,3.2,6.2));
#12141=CARTESIAN_POINT('',(-2.,3.2,2.8));
#12142=CARTESIAN_POINT('',(0.,3.2,6.2));
#12143=CARTESIAN_POINT('',(0.,3.2,6.2));
#12144=CARTESIAN_POINT('',(0.,3.2,2.8));
#12145=CARTESIAN_POINT('Origin',(0.,-3.2,2.8));
#12146=CARTESIAN_POINT('',(0.,-3.2,2.8));
#12147=CARTESIAN_POINT('',(0.,-3.2,2.8));
#12148=CARTESIAN_POINT('',(0.,-3.2,6.2));
#12149=CARTESIAN_POINT('',(0.,-3.2,6.2));
#12150=CARTESIAN_POINT('',(0.,-3.2,2.8));
#12151=CARTESIAN_POINT('Origin',(-2.,-3.2,2.8));
#12152=CARTESIAN_POINT('',(-2.,-3.2,2.8));
#12153=CARTESIAN_POINT('',(-2.,-3.2,2.8));
#12154=CARTESIAN_POINT('',(-2.,-3.2,6.2));
#12155=CARTESIAN_POINT('',(-2.,-3.2,6.2));
#12156=CARTESIAN_POINT('',(-2.,-3.2,2.8));
#12157=CARTESIAN_POINT('Origin',(-2.,3.2,2.8));
#12158=CARTESIAN_POINT('',(-2.,3.2,2.8));
#12159=CARTESIAN_POINT('',(-2.,3.2,6.2));
#12160=CARTESIAN_POINT('Origin',(-1.,0.,6.2));
#12161=CARTESIAN_POINT('Origin',(-1.,0.,2.8));
#12162=CARTESIAN_POINT('',(0.,0.,0.));
#12163=CARTESIAN_POINT('Origin',(0.2,3.,5.2));
#12164=CARTESIAN_POINT('',(0.2,3.,5.2));
#12165=CARTESIAN_POINT('',(0.,3.,5.2));
#12166=CARTESIAN_POINT('',(0.2,3.,5.2));
#12167=CARTESIAN_POINT('',(0.,3.,6.2));
#12168=CARTESIAN_POINT('',(0.,3.,5.2));
#12169=CARTESIAN_POINT('',(0.2,3.,6.2));
#12170=CARTESIAN_POINT('',(0.2,3.,6.2));
#12171=CARTESIAN_POINT('',(0.2,3.,5.2));
#12172=CARTESIAN_POINT('Origin',(0.2,-3.,5.2));
#12173=CARTESIAN_POINT('',(0.2,-3.,5.2));
#12174=CARTESIAN_POINT('',(0.2,-3.,5.2));
#12175=CARTESIAN_POINT('',(0.2,-3.,6.2));
#12176=CARTESIAN_POINT('',(0.2,-3.,6.2));
#12177=CARTESIAN_POINT('',(0.2,-3.,5.2));
#12178=CARTESIAN_POINT('Origin',(0.,-3.,5.2));
#12179=CARTESIAN_POINT('',(0.,-3.,5.2));
#12180=CARTESIAN_POINT('',(0.,-3.,5.2));
#12181=CARTESIAN_POINT('',(0.,-3.,6.2));
#12182=CARTESIAN_POINT('',(0.,-3.,6.2));
#12183=CARTESIAN_POINT('',(0.,-3.,5.2));
#12184=CARTESIAN_POINT('Origin',(0.,3.,5.2));
#12185=CARTESIAN_POINT('',(0.,3.,5.2));
#12186=CARTESIAN_POINT('',(0.,3.,6.2));
#12187=CARTESIAN_POINT('Origin',(0.1,0.,6.2));
#12188=CARTESIAN_POINT('Origin',(0.1,0.,5.2));
#12189=CARTESIAN_POINT('',(0.,0.,0.));
#12190=CARTESIAN_POINT('Origin',(23.,-2.4,4.));
#12191=CARTESIAN_POINT('',(22.525,-2.4,4.));
#12192=CARTESIAN_POINT('Origin',(23.,-2.4,4.));
#12193=CARTESIAN_POINT('',(22.525,-2.4,6.2));
#12194=CARTESIAN_POINT('',(22.525,-2.4,4.));
#12195=CARTESIAN_POINT('Origin',(23.,-2.4,6.2));
#12196=CARTESIAN_POINT('Origin',(23.,-2.4,4.));
#12197=CARTESIAN_POINT('',(22.725,-2.4,4.));
#12198=CARTESIAN_POINT('Origin',(23.,-2.4,4.));
#12199=CARTESIAN_POINT('Origin',(23.,2.4,4.));
#12200=CARTESIAN_POINT('',(22.525,2.4,4.));
#12201=CARTESIAN_POINT('Origin',(23.,2.4,4.));
#12202=CARTESIAN_POINT('',(22.525,2.4,6.2));
#12203=CARTESIAN_POINT('',(22.525,2.4,4.));
#12204=CARTESIAN_POINT('Origin',(23.,2.4,6.2));
#12205=CARTESIAN_POINT('Origin',(23.,2.4,4.));
#12206=CARTESIAN_POINT('',(22.725,2.4,4.));
#12207=CARTESIAN_POINT('Origin',(23.,2.4,4.));
#12208=CARTESIAN_POINT('Origin',(23.,-2.4,2.7));
#12209=CARTESIAN_POINT('',(22.725,-2.4,2.8));
#12210=CARTESIAN_POINT('Origin',(23.,-2.4,2.8));
#12211=CARTESIAN_POINT('',(22.725,-2.4,2.7));
#12212=CARTESIAN_POINT('Origin',(23.,2.4,2.7));
#12213=CARTESIAN_POINT('',(22.725,2.4,2.8));
#12214=CARTESIAN_POINT('Origin',(23.,2.4,2.8));
#12215=CARTESIAN_POINT('',(22.725,2.4,2.7));
#12216=CARTESIAN_POINT('Origin',(24.,3.2,2.8));
#12217=CARTESIAN_POINT('',(24.,3.2,2.8));
#12218=CARTESIAN_POINT('',(22.,3.2,2.8));
#12219=CARTESIAN_POINT('',(24.,3.2,2.8));
#12220=CARTESIAN_POINT('',(22.,3.2,6.2));
#12221=CARTESIAN_POINT('',(22.,3.2,2.8));
#12222=CARTESIAN_POINT('',(24.,3.2,6.2));
#12223=CARTESIAN_POINT('',(24.,3.2,6.2));
#12224=CARTESIAN_POINT('',(24.,3.2,2.8));
#12225=CARTESIAN_POINT('Origin',(24.,-3.2,2.8));
#12226=CARTESIAN_POINT('',(24.,-3.2,2.8));
#12227=CARTESIAN_POINT('',(24.,-3.2,2.8));
#12228=CARTESIAN_POINT('',(24.,-3.2,6.2));
#12229=CARTESIAN_POINT('',(24.,-3.2,6.2));
#12230=CARTESIAN_POINT('',(24.,-3.2,2.8));
#12231=CARTESIAN_POINT('Origin',(22.,-3.2,2.8));
#12232=CARTESIAN_POINT('',(22.,-3.2,2.8));
#12233=CARTESIAN_POINT('',(22.,-3.2,2.8));
#12234=CARTESIAN_POINT('',(22.,-3.2,6.2));
#12235=CARTESIAN_POINT('',(22.,-3.2,6.2));
#12236=CARTESIAN_POINT('',(22.,-3.2,2.8));
#12237=CARTESIAN_POINT('Origin',(22.,3.2,2.8));
#12238=CARTESIAN_POINT('',(22.,3.2,2.8));
#12239=CARTESIAN_POINT('',(22.,3.2,6.2));
#12240=CARTESIAN_POINT('Origin',(23.,0.,6.2));
#12241=CARTESIAN_POINT('Origin',(23.,0.,2.8));
#12242=CARTESIAN_POINT('',(0.,0.,0.));
#12243=CARTESIAN_POINT('Origin',(22.,3.,5.2));
#12244=CARTESIAN_POINT('',(22.,3.,5.2));
#12245=CARTESIAN_POINT('',(21.8,3.,5.2));
#12246=CARTESIAN_POINT('',(22.,3.,5.2));
#12247=CARTESIAN_POINT('',(21.8,3.,6.2));
#12248=CARTESIAN_POINT('',(21.8,3.,5.2));
#12249=CARTESIAN_POINT('',(22.,3.,6.2));
#12250=CARTESIAN_POINT('',(22.,3.,6.2));
#12251=CARTESIAN_POINT('',(22.,3.,5.2));
#12252=CARTESIAN_POINT('Origin',(22.,-3.,5.2));
#12253=CARTESIAN_POINT('',(22.,-3.,5.2));
#12254=CARTESIAN_POINT('',(22.,-3.,5.2));
#12255=CARTESIAN_POINT('',(22.,-3.,6.2));
#12256=CARTESIAN_POINT('',(22.,-3.,6.2));
#12257=CARTESIAN_POINT('',(22.,-3.,5.2));
#12258=CARTESIAN_POINT('Origin',(21.8,-3.,5.2));
#12259=CARTESIAN_POINT('',(21.8,-3.,5.2));
#12260=CARTESIAN_POINT('',(21.8,-3.,5.2));
#12261=CARTESIAN_POINT('',(21.8,-3.,6.2));
#12262=CARTESIAN_POINT('',(21.8,-3.,6.2));
#12263=CARTESIAN_POINT('',(21.8,-3.,5.2));
#12264=CARTESIAN_POINT('Origin',(21.8,3.,5.2));
#12265=CARTESIAN_POINT('',(21.8,3.,5.2));
#12266=CARTESIAN_POINT('',(21.8,3.,6.2));
#12267=CARTESIAN_POINT('Origin',(21.9,0.,6.2));
#12268=CARTESIAN_POINT('Origin',(21.9,0.,5.2));
#12269=CARTESIAN_POINT('',(0.,0.,0.));
#12270=CARTESIAN_POINT('Origin',(17.51,4.3,2.98));
#12271=CARTESIAN_POINT('',(17.51,4.3,2.98));
#12272=CARTESIAN_POINT('',(17.49,4.3,2.98));
#12273=CARTESIAN_POINT('',(17.51,4.3,2.98));
#12274=CARTESIAN_POINT('',(17.51,4.3,3.));
#12275=CARTESIAN_POINT('',(17.51,4.3,2.98));
#12276=CARTESIAN_POINT('',(17.49,4.3,3.));
#12277=CARTESIAN_POINT('',(14.255,4.3,3.));
#12278=CARTESIAN_POINT('',(17.49,4.3,2.98));
#12279=CARTESIAN_POINT('Origin',(17.51,4.,2.98));
#12280=CARTESIAN_POINT('',(17.51,4.,2.98));
#12281=CARTESIAN_POINT('',(17.51,4.,2.98));
#12282=CARTESIAN_POINT('',(17.51,4.,3.));
#12283=CARTESIAN_POINT('',(17.51,4.,2.89));
#12284=CARTESIAN_POINT('',(17.51,4.2,3.));
#12285=CARTESIAN_POINT('Origin',(17.49,4.3,2.98));
#12286=CARTESIAN_POINT('',(17.49,4.,2.98));
#12287=CARTESIAN_POINT('',(17.49,4.3,2.98));
#12288=CARTESIAN_POINT('',(17.49,4.,3.));
#12289=CARTESIAN_POINT('',(17.49,4.35,3.));
#12290=CARTESIAN_POINT('',(17.49,4.,2.89));
#12291=CARTESIAN_POINT('Origin',(17.5,4.15,2.98));
#12292=CARTESIAN_POINT('',(9.25,4.,2.98));
#12293=CARTESIAN_POINT('Origin',(16.51,4.3,2.98));
#12294=CARTESIAN_POINT('',(16.51,4.3,2.98));
#12295=CARTESIAN_POINT('',(16.49,4.3,2.98));
#12296=CARTESIAN_POINT('',(16.51,4.3,2.98));
#12297=CARTESIAN_POINT('',(16.51,4.3,3.));
#12298=CARTESIAN_POINT('',(16.51,4.3,2.98));
#12299=CARTESIAN_POINT('',(16.49,4.3,3.));
#12300=CARTESIAN_POINT('',(13.755,4.3,3.));
#12301=CARTESIAN_POINT('',(16.49,4.3,2.98));
#12302=CARTESIAN_POINT('Origin',(16.51,4.,2.98));
#12303=CARTESIAN_POINT('',(16.51,4.,2.98));
#12304=CARTESIAN_POINT('',(16.51,4.,2.98));
#12305=CARTESIAN_POINT('',(16.51,4.,3.));
#12306=CARTESIAN_POINT('',(16.51,4.,2.89));
#12307=CARTESIAN_POINT('',(16.51,4.2,3.));
#12308=CARTESIAN_POINT('Origin',(16.49,4.3,2.98));
#12309=CARTESIAN_POINT('',(16.49,4.,2.98));
#12310=CARTESIAN_POINT('',(16.49,4.3,2.98));
#12311=CARTESIAN_POINT('',(16.49,4.,3.));
#12312=CARTESIAN_POINT('',(16.49,4.35,3.));
#12313=CARTESIAN_POINT('',(16.49,4.,2.89));
#12314=CARTESIAN_POINT('Origin',(16.5,4.15,2.98));
#12315=CARTESIAN_POINT('',(8.75,4.,2.98));
#12316=CARTESIAN_POINT('Origin',(15.51,4.3,2.98));
#12317=CARTESIAN_POINT('',(15.51,4.3,2.98));
#12318=CARTESIAN_POINT('',(15.49,4.3,2.98));
#12319=CARTESIAN_POINT('',(15.51,4.3,2.98));
#12320=CARTESIAN_POINT('',(15.51,4.3,3.));
#12321=CARTESIAN_POINT('',(15.51,4.3,2.98));
#12322=CARTESIAN_POINT('',(15.49,4.3,3.));
#12323=CARTESIAN_POINT('',(13.255,4.3,3.));
#12324=CARTESIAN_POINT('',(15.49,4.3,2.98));
#12325=CARTESIAN_POINT('Origin',(15.51,4.,2.98));
#12326=CARTESIAN_POINT('',(15.51,4.,2.98));
#12327=CARTESIAN_POINT('',(15.51,4.,2.98));
#12328=CARTESIAN_POINT('',(15.51,4.,3.));
#12329=CARTESIAN_POINT('',(15.51,4.,2.89));
#12330=CARTESIAN_POINT('',(15.51,4.2,3.));
#12331=CARTESIAN_POINT('Origin',(15.49,4.3,2.98));
#12332=CARTESIAN_POINT('',(15.49,4.,2.98));
#12333=CARTESIAN_POINT('',(15.49,4.3,2.98));
#12334=CARTESIAN_POINT('',(15.49,4.,3.));
#12335=CARTESIAN_POINT('',(15.49,4.35,3.));
#12336=CARTESIAN_POINT('',(15.49,4.,2.89));
#12337=CARTESIAN_POINT('Origin',(15.5,4.15,2.98));
#12338=CARTESIAN_POINT('',(8.25,4.,2.98));
#12339=CARTESIAN_POINT('Origin',(14.51,4.3,2.98));
#12340=CARTESIAN_POINT('',(14.51,4.3,2.98));
#12341=CARTESIAN_POINT('',(14.49,4.3,2.98));
#12342=CARTESIAN_POINT('',(14.51,4.3,2.98));
#12343=CARTESIAN_POINT('',(14.51,4.3,3.));
#12344=CARTESIAN_POINT('',(14.51,4.3,2.98));
#12345=CARTESIAN_POINT('',(14.49,4.3,3.));
#12346=CARTESIAN_POINT('',(12.755,4.3,3.));
#12347=CARTESIAN_POINT('',(14.49,4.3,2.98));
#12348=CARTESIAN_POINT('Origin',(14.51,4.,2.98));
#12349=CARTESIAN_POINT('',(14.51,4.,2.98));
#12350=CARTESIAN_POINT('',(14.51,4.,2.98));
#12351=CARTESIAN_POINT('',(14.51,4.,3.));
#12352=CARTESIAN_POINT('',(14.51,4.,2.89));
#12353=CARTESIAN_POINT('',(14.51,4.2,3.));
#12354=CARTESIAN_POINT('Origin',(14.49,4.3,2.98));
#12355=CARTESIAN_POINT('',(14.49,4.,2.98));
#12356=CARTESIAN_POINT('',(14.49,4.3,2.98));
#12357=CARTESIAN_POINT('',(14.49,4.,3.));
#12358=CARTESIAN_POINT('',(14.49,4.35,3.));
#12359=CARTESIAN_POINT('',(14.49,4.,2.89));
#12360=CARTESIAN_POINT('Origin',(14.5,4.15,2.98));
#12361=CARTESIAN_POINT('',(7.75,4.,2.98));
#12362=CARTESIAN_POINT('Origin',(13.51,4.3,2.98));
#12363=CARTESIAN_POINT('',(13.51,4.3,2.98));
#12364=CARTESIAN_POINT('',(13.49,4.3,2.98));
#12365=CARTESIAN_POINT('',(13.51,4.3,2.98));
#12366=CARTESIAN_POINT('',(13.51,4.3,3.));
#12367=CARTESIAN_POINT('',(13.51,4.3,2.98));
#12368=CARTESIAN_POINT('',(13.49,4.3,3.));
#12369=CARTESIAN_POINT('',(12.255,4.3,3.));
#12370=CARTESIAN_POINT('',(13.49,4.3,2.98));
#12371=CARTESIAN_POINT('Origin',(13.51,4.,2.98));
#12372=CARTESIAN_POINT('',(13.51,4.,2.98));
#12373=CARTESIAN_POINT('',(13.51,4.,2.98));
#12374=CARTESIAN_POINT('',(13.51,4.,3.));
#12375=CARTESIAN_POINT('',(13.51,4.,2.89));
#12376=CARTESIAN_POINT('',(13.51,4.2,3.));
#12377=CARTESIAN_POINT('Origin',(13.49,4.3,2.98));
#12378=CARTESIAN_POINT('',(13.49,4.,2.98));
#12379=CARTESIAN_POINT('',(13.49,4.3,2.98));
#12380=CARTESIAN_POINT('',(13.49,4.,3.));
#12381=CARTESIAN_POINT('',(13.49,4.35,3.));
#12382=CARTESIAN_POINT('',(13.49,4.,2.89));
#12383=CARTESIAN_POINT('Origin',(13.5,4.15,2.98));
#12384=CARTESIAN_POINT('',(7.25,4.,2.98));
#12385=CARTESIAN_POINT('Origin',(12.51,4.3,2.98));
#12386=CARTESIAN_POINT('',(12.51,4.3,2.98));
#12387=CARTESIAN_POINT('',(12.49,4.3,2.98));
#12388=CARTESIAN_POINT('',(12.51,4.3,2.98));
#12389=CARTESIAN_POINT('',(12.51,4.3,3.));
#12390=CARTESIAN_POINT('',(12.51,4.3,2.98));
#12391=CARTESIAN_POINT('',(12.49,4.3,3.));
#12392=CARTESIAN_POINT('',(11.755,4.3,3.));
#12393=CARTESIAN_POINT('',(12.49,4.3,2.98));
#12394=CARTESIAN_POINT('Origin',(12.51,4.,2.98));
#12395=CARTESIAN_POINT('',(12.51,4.,2.98));
#12396=CARTESIAN_POINT('',(12.51,4.,2.98));
#12397=CARTESIAN_POINT('',(12.51,4.,3.));
#12398=CARTESIAN_POINT('',(12.51,4.,2.89));
#12399=CARTESIAN_POINT('',(12.51,4.2,3.));
#12400=CARTESIAN_POINT('Origin',(12.49,4.3,2.98));
#12401=CARTESIAN_POINT('',(12.49,4.,2.98));
#12402=CARTESIAN_POINT('',(12.49,4.3,2.98));
#12403=CARTESIAN_POINT('',(12.49,4.,3.));
#12404=CARTESIAN_POINT('',(12.49,4.35,3.));
#12405=CARTESIAN_POINT('',(12.49,4.,2.89));
#12406=CARTESIAN_POINT('Origin',(12.5,4.15,2.98));
#12407=CARTESIAN_POINT('',(6.75,4.,2.98));
#12408=CARTESIAN_POINT('Origin',(11.51,4.3,2.98));
#12409=CARTESIAN_POINT('',(11.51,4.3,2.98));
#12410=CARTESIAN_POINT('',(11.49,4.3,2.98));
#12411=CARTESIAN_POINT('',(11.51,4.3,2.98));
#12412=CARTESIAN_POINT('',(11.51,4.3,3.));
#12413=CARTESIAN_POINT('',(11.51,4.3,2.98));
#12414=CARTESIAN_POINT('',(11.49,4.3,3.));
#12415=CARTESIAN_POINT('',(11.255,4.3,3.));
#12416=CARTESIAN_POINT('',(11.49,4.3,2.98));
#12417=CARTESIAN_POINT('Origin',(11.51,4.,2.98));
#12418=CARTESIAN_POINT('',(11.51,4.,2.98));
#12419=CARTESIAN_POINT('',(11.51,4.,2.98));
#12420=CARTESIAN_POINT('',(11.51,4.,3.));
#12421=CARTESIAN_POINT('',(11.51,4.,2.89));
#12422=CARTESIAN_POINT('',(11.51,4.2,3.));
#12423=CARTESIAN_POINT('Origin',(11.49,4.3,2.98));
#12424=CARTESIAN_POINT('',(11.49,4.,2.98));
#12425=CARTESIAN_POINT('',(11.49,4.3,2.98));
#12426=CARTESIAN_POINT('',(11.49,4.,3.));
#12427=CARTESIAN_POINT('',(11.49,4.35,3.));
#12428=CARTESIAN_POINT('',(11.49,4.,2.89));
#12429=CARTESIAN_POINT('Origin',(11.5,4.15,2.98));
#12430=CARTESIAN_POINT('',(6.25,4.,2.98));
#12431=CARTESIAN_POINT('Origin',(11.01,4.5,2.98));
#12432=CARTESIAN_POINT('',(11.01,4.5,2.98));
#12433=CARTESIAN_POINT('',(10.99,4.5,2.98));
#12434=CARTESIAN_POINT('',(11.01,4.5,2.98));
#12435=CARTESIAN_POINT('',(11.01,4.5,3.));
#12436=CARTESIAN_POINT('',(11.01,4.5,2.98));
#12437=CARTESIAN_POINT('',(10.99,4.5,3.));
#12438=CARTESIAN_POINT('',(11.005,4.5,3.));
#12439=CARTESIAN_POINT('',(10.99,4.5,2.98));
#12440=CARTESIAN_POINT('Origin',(11.01,4.,2.98));
#12441=CARTESIAN_POINT('',(11.01,4.,2.98));
#12442=CARTESIAN_POINT('',(11.01,4.,2.98));
#12443=CARTESIAN_POINT('',(11.01,4.,3.));
#12444=CARTESIAN_POINT('',(11.01,4.,2.89));
#12445=CARTESIAN_POINT('',(11.01,4.2,3.));
#12446=CARTESIAN_POINT('Origin',(10.99,4.5,2.98));
#12447=CARTESIAN_POINT('',(10.99,4.,2.98));
#12448=CARTESIAN_POINT('',(10.99,4.5,2.98));
#12449=CARTESIAN_POINT('',(10.99,4.,3.));
#12450=CARTESIAN_POINT('',(10.99,4.45,3.));
#12451=CARTESIAN_POINT('',(10.99,4.,2.89));
#12452=CARTESIAN_POINT('Origin',(11.,4.25,2.98));
#12453=CARTESIAN_POINT('',(6.,4.,2.98));
#12454=CARTESIAN_POINT('Origin',(10.01,4.5,2.98));
#12455=CARTESIAN_POINT('',(10.01,4.5,2.98));
#12456=CARTESIAN_POINT('',(9.99,4.5,2.98));
#12457=CARTESIAN_POINT('',(10.01,4.5,2.98));
#12458=CARTESIAN_POINT('',(10.01,4.5,3.));
#12459=CARTESIAN_POINT('',(10.01,4.5,2.98));
#12460=CARTESIAN_POINT('',(9.99,4.5,3.));
#12461=CARTESIAN_POINT('',(10.505,4.5,3.));
#12462=CARTESIAN_POINT('',(9.99,4.5,2.98));
#12463=CARTESIAN_POINT('Origin',(10.01,4.,2.98));
#12464=CARTESIAN_POINT('',(10.01,4.,2.98));
#12465=CARTESIAN_POINT('',(10.01,4.,2.98));
#12466=CARTESIAN_POINT('',(10.01,4.,3.));
#12467=CARTESIAN_POINT('',(10.01,4.,2.89));
#12468=CARTESIAN_POINT('',(10.01,4.2,3.));
#12469=CARTESIAN_POINT('Origin',(9.99,4.5,2.98));
#12470=CARTESIAN_POINT('',(9.99,4.,2.98));
#12471=CARTESIAN_POINT('',(9.99,4.5,2.98));
#12472=CARTESIAN_POINT('',(9.99,4.,3.));
#12473=CARTESIAN_POINT('',(9.99,4.45,3.));
#12474=CARTESIAN_POINT('',(9.99,4.,2.89));
#12475=CARTESIAN_POINT('Origin',(10.,4.25,2.98));
#12476=CARTESIAN_POINT('',(5.5,4.,2.98));
#12477=CARTESIAN_POINT('Origin',(9.01,4.5,2.98));
#12478=CARTESIAN_POINT('',(9.01,4.5,2.98));
#12479=CARTESIAN_POINT('',(8.99,4.5,2.98));
#12480=CARTESIAN_POINT('',(9.01,4.5,2.98));
#12481=CARTESIAN_POINT('',(9.01,4.5,3.));
#12482=CARTESIAN_POINT('',(9.01,4.5,2.98));
#12483=CARTESIAN_POINT('',(8.99,4.5,3.));
#12484=CARTESIAN_POINT('',(10.005,4.5,3.));
#12485=CARTESIAN_POINT('',(8.99,4.5,2.98));
#12486=CARTESIAN_POINT('Origin',(9.01,4.,2.98));
#12487=CARTESIAN_POINT('',(9.01,4.,2.98));
#12488=CARTESIAN_POINT('',(9.01,4.,2.98));
#12489=CARTESIAN_POINT('',(9.01,4.,3.));
#12490=CARTESIAN_POINT('',(9.01,4.,2.89));
#12491=CARTESIAN_POINT('',(9.01,4.2,3.));
#12492=CARTESIAN_POINT('Origin',(8.99,4.5,2.98));
#12493=CARTESIAN_POINT('',(8.99,4.,2.98));
#12494=CARTESIAN_POINT('',(8.99,4.5,2.98));
#12495=CARTESIAN_POINT('',(8.99,4.,3.));
#12496=CARTESIAN_POINT('',(8.99,4.45,3.));
#12497=CARTESIAN_POINT('',(8.99,4.,2.89));
#12498=CARTESIAN_POINT('Origin',(9.,4.25,2.98));
#12499=CARTESIAN_POINT('',(5.,4.,2.98));
#12500=CARTESIAN_POINT('Origin',(8.01,4.5,2.98));
#12501=CARTESIAN_POINT('',(8.01,4.5,2.98));
#12502=CARTESIAN_POINT('',(7.99,4.5,2.98));
#12503=CARTESIAN_POINT('',(8.01,4.5,2.98));
#12504=CARTESIAN_POINT('',(8.01,4.5,3.));
#12505=CARTESIAN_POINT('',(8.01,4.5,2.98));
#12506=CARTESIAN_POINT('',(7.99,4.5,3.));
#12507=CARTESIAN_POINT('',(9.505,4.5,3.));
#12508=CARTESIAN_POINT('',(7.99,4.5,2.98));
#12509=CARTESIAN_POINT('Origin',(8.01,4.,2.98));
#12510=CARTESIAN_POINT('',(8.01,4.,2.98));
#12511=CARTESIAN_POINT('',(8.01,4.,2.98));
#12512=CARTESIAN_POINT('',(8.01,4.,3.));
#12513=CARTESIAN_POINT('',(8.01,4.,2.89));
#12514=CARTESIAN_POINT('',(8.01,4.2,3.));
#12515=CARTESIAN_POINT('Origin',(7.99,4.5,2.98));
#12516=CARTESIAN_POINT('',(7.99,4.,2.98));
#12517=CARTESIAN_POINT('',(7.99,4.5,2.98));
#12518=CARTESIAN_POINT('',(7.99,4.,3.));
#12519=CARTESIAN_POINT('',(7.99,4.45,3.));
#12520=CARTESIAN_POINT('',(7.99,4.,2.89));
#12521=CARTESIAN_POINT('Origin',(8.,4.25,2.98));
#12522=CARTESIAN_POINT('',(4.5,4.,2.98));
#12523=CARTESIAN_POINT('Origin',(7.01,4.5,2.98));
#12524=CARTESIAN_POINT('',(7.01,4.5,2.98));
#12525=CARTESIAN_POINT('',(6.99,4.5,2.98));
#12526=CARTESIAN_POINT('',(7.01,4.5,2.98));
#12527=CARTESIAN_POINT('',(7.01,4.5,3.));
#12528=CARTESIAN_POINT('',(7.01,4.5,2.98));
#12529=CARTESIAN_POINT('',(6.99,4.5,3.));
#12530=CARTESIAN_POINT('',(9.005,4.5,3.));
#12531=CARTESIAN_POINT('',(6.99,4.5,2.98));
#12532=CARTESIAN_POINT('Origin',(7.01,4.,2.98));
#12533=CARTESIAN_POINT('',(7.01,4.,2.98));
#12534=CARTESIAN_POINT('',(7.01,4.,2.98));
#12535=CARTESIAN_POINT('',(7.01,4.,3.));
#12536=CARTESIAN_POINT('',(7.01,4.,2.89));
#12537=CARTESIAN_POINT('',(7.01,4.2,3.));
#12538=CARTESIAN_POINT('Origin',(6.99,4.5,2.98));
#12539=CARTESIAN_POINT('',(6.99,4.,2.98));
#12540=CARTESIAN_POINT('',(6.99,4.5,2.98));
#12541=CARTESIAN_POINT('',(6.99,4.,3.));
#12542=CARTESIAN_POINT('',(6.99,4.45,3.));
#12543=CARTESIAN_POINT('',(6.99,4.,2.89));
#12544=CARTESIAN_POINT('Origin',(7.,4.25,2.98));
#12545=CARTESIAN_POINT('',(4.,4.,2.98));
#12546=CARTESIAN_POINT('Origin',(6.01,4.5,2.98));
#12547=CARTESIAN_POINT('',(6.01,4.5,2.98));
#12548=CARTESIAN_POINT('',(5.99,4.5,2.98));
#12549=CARTESIAN_POINT('',(6.01,4.5,2.98));
#12550=CARTESIAN_POINT('',(6.01,4.5,3.));
#12551=CARTESIAN_POINT('',(6.01,4.5,2.98));
#12552=CARTESIAN_POINT('',(5.99,4.5,3.));
#12553=CARTESIAN_POINT('',(8.505,4.5,3.));
#12554=CARTESIAN_POINT('',(5.99,4.5,2.98));
#12555=CARTESIAN_POINT('Origin',(6.01,4.,2.98));
#12556=CARTESIAN_POINT('',(6.01,4.,2.98));
#12557=CARTESIAN_POINT('',(6.01,4.,2.98));
#12558=CARTESIAN_POINT('',(6.01,4.,3.));
#12559=CARTESIAN_POINT('',(6.01,4.,2.89));
#12560=CARTESIAN_POINT('',(6.01,4.2,3.));
#12561=CARTESIAN_POINT('Origin',(5.99,4.5,2.98));
#12562=CARTESIAN_POINT('',(5.99,4.,2.98));
#12563=CARTESIAN_POINT('',(5.99,4.5,2.98));
#12564=CARTESIAN_POINT('',(5.99,4.,3.));
#12565=CARTESIAN_POINT('',(5.99,4.45,3.));
#12566=CARTESIAN_POINT('',(5.99,4.,2.89));
#12567=CARTESIAN_POINT('Origin',(6.,4.25,2.98));
#12568=CARTESIAN_POINT('',(3.5,4.,2.98));
#12569=CARTESIAN_POINT('Origin',(5.01,4.5,2.98));
#12570=CARTESIAN_POINT('',(5.01,4.5,2.98));
#12571=CARTESIAN_POINT('',(4.99,4.5,2.98));
#12572=CARTESIAN_POINT('',(5.01,4.5,2.98));
#12573=CARTESIAN_POINT('',(5.01,4.5,3.));
#12574=CARTESIAN_POINT('',(5.01,4.5,2.98));
#12575=CARTESIAN_POINT('',(4.99,4.5,3.));
#12576=CARTESIAN_POINT('',(8.005,4.5,3.));
#12577=CARTESIAN_POINT('',(4.99,4.5,2.98));
#12578=CARTESIAN_POINT('Origin',(5.01,4.,2.98));
#12579=CARTESIAN_POINT('',(5.01,4.,2.98));
#12580=CARTESIAN_POINT('',(5.01,4.,2.98));
#12581=CARTESIAN_POINT('',(5.01,4.,3.));
#12582=CARTESIAN_POINT('',(5.01,4.,2.89));
#12583=CARTESIAN_POINT('',(5.01,4.2,3.));
#12584=CARTESIAN_POINT('Origin',(4.99,4.5,2.98));
#12585=CARTESIAN_POINT('',(4.99,4.,2.98));
#12586=CARTESIAN_POINT('',(4.99,4.5,2.98));
#12587=CARTESIAN_POINT('',(4.99,4.,3.));
#12588=CARTESIAN_POINT('',(4.99,4.45,3.));
#12589=CARTESIAN_POINT('',(4.99,4.,2.89));
#12590=CARTESIAN_POINT('Origin',(5.,4.25,2.98));
#12591=CARTESIAN_POINT('',(3.,4.,2.98));
#12592=CARTESIAN_POINT('Origin',(4.51,4.3,2.98));
#12593=CARTESIAN_POINT('',(4.51,4.3,2.98));
#12594=CARTESIAN_POINT('',(4.49,4.3,2.98));
#12595=CARTESIAN_POINT('',(4.51,4.3,2.98));
#12596=CARTESIAN_POINT('',(4.51,4.3,3.));
#12597=CARTESIAN_POINT('',(4.51,4.3,2.98));
#12598=CARTESIAN_POINT('',(4.49,4.3,3.));
#12599=CARTESIAN_POINT('',(7.755,4.3,3.));
#12600=CARTESIAN_POINT('',(4.49,4.3,2.98));
#12601=CARTESIAN_POINT('Origin',(4.51,4.,2.98));
#12602=CARTESIAN_POINT('',(4.51,4.,2.98));
#12603=CARTESIAN_POINT('',(4.51,4.,2.98));
#12604=CARTESIAN_POINT('',(4.51,4.,3.));
#12605=CARTESIAN_POINT('',(4.51,4.,2.89));
#12606=CARTESIAN_POINT('',(4.51,4.2,3.));
#12607=CARTESIAN_POINT('Origin',(4.49,4.3,2.98));
#12608=CARTESIAN_POINT('',(4.49,4.,2.98));
#12609=CARTESIAN_POINT('',(4.49,4.3,2.98));
#12610=CARTESIAN_POINT('',(4.49,4.,3.));
#12611=CARTESIAN_POINT('',(4.49,4.35,3.));
#12612=CARTESIAN_POINT('',(4.49,4.,2.89));
#12613=CARTESIAN_POINT('Origin',(4.5,4.15,2.98));
#12614=CARTESIAN_POINT('',(2.75,4.,2.98));
#12615=CARTESIAN_POINT('Origin',(5.51,4.3,2.98));
#12616=CARTESIAN_POINT('',(5.51,4.3,2.98));
#12617=CARTESIAN_POINT('',(5.49,4.3,2.98));
#12618=CARTESIAN_POINT('',(5.51,4.3,2.98));
#12619=CARTESIAN_POINT('',(5.51,4.3,3.));
#12620=CARTESIAN_POINT('',(5.51,4.3,2.98));
#12621=CARTESIAN_POINT('',(5.49,4.3,3.));
#12622=CARTESIAN_POINT('',(8.255,4.3,3.));
#12623=CARTESIAN_POINT('',(5.49,4.3,2.98));
#12624=CARTESIAN_POINT('Origin',(5.51,4.,2.98));
#12625=CARTESIAN_POINT('',(5.51,4.,2.98));
#12626=CARTESIAN_POINT('',(5.51,4.,2.98));
#12627=CARTESIAN_POINT('',(5.51,4.,3.));
#12628=CARTESIAN_POINT('',(5.51,4.,2.89));
#12629=CARTESIAN_POINT('',(5.51,4.2,3.));
#12630=CARTESIAN_POINT('Origin',(5.49,4.3,2.98));
#12631=CARTESIAN_POINT('',(5.49,4.,2.98));
#12632=CARTESIAN_POINT('',(5.49,4.3,2.98));
#12633=CARTESIAN_POINT('',(5.49,4.,3.));
#12634=CARTESIAN_POINT('',(5.49,4.35,3.));
#12635=CARTESIAN_POINT('',(5.49,4.,2.89));
#12636=CARTESIAN_POINT('Origin',(5.5,4.15,2.98));
#12637=CARTESIAN_POINT('',(3.25,4.,2.98));
#12638=CARTESIAN_POINT('Origin',(6.51,4.3,2.98));
#12639=CARTESIAN_POINT('',(6.51,4.3,2.98));
#12640=CARTESIAN_POINT('',(6.49,4.3,2.98));
#12641=CARTESIAN_POINT('',(6.51,4.3,2.98));
#12642=CARTESIAN_POINT('',(6.51,4.3,3.));
#12643=CARTESIAN_POINT('',(6.51,4.3,2.98));
#12644=CARTESIAN_POINT('',(6.49,4.3,3.));
#12645=CARTESIAN_POINT('',(8.755,4.3,3.));
#12646=CARTESIAN_POINT('',(6.49,4.3,2.98));
#12647=CARTESIAN_POINT('Origin',(6.51,4.,2.98));
#12648=CARTESIAN_POINT('',(6.51,4.,2.98));
#12649=CARTESIAN_POINT('',(6.51,4.,2.98));
#12650=CARTESIAN_POINT('',(6.51,4.,3.));
#12651=CARTESIAN_POINT('',(6.51,4.,2.89));
#12652=CARTESIAN_POINT('',(6.51,4.2,3.));
#12653=CARTESIAN_POINT('Origin',(6.49,4.3,2.98));
#12654=CARTESIAN_POINT('',(6.49,4.,2.98));
#12655=CARTESIAN_POINT('',(6.49,4.3,2.98));
#12656=CARTESIAN_POINT('',(6.49,4.,3.));
#12657=CARTESIAN_POINT('',(6.49,4.35,3.));
#12658=CARTESIAN_POINT('',(6.49,4.,2.89));
#12659=CARTESIAN_POINT('Origin',(6.5,4.15,2.98));
#12660=CARTESIAN_POINT('',(3.75,4.,2.98));
#12661=CARTESIAN_POINT('Origin',(7.51,4.3,2.98));
#12662=CARTESIAN_POINT('',(7.51,4.3,2.98));
#12663=CARTESIAN_POINT('',(7.49,4.3,2.98));
#12664=CARTESIAN_POINT('',(7.51,4.3,2.98));
#12665=CARTESIAN_POINT('',(7.51,4.3,3.));
#12666=CARTESIAN_POINT('',(7.51,4.3,2.98));
#12667=CARTESIAN_POINT('',(7.49,4.3,3.));
#12668=CARTESIAN_POINT('',(9.255,4.3,3.));
#12669=CARTESIAN_POINT('',(7.49,4.3,2.98));
#12670=CARTESIAN_POINT('Origin',(7.51,4.,2.98));
#12671=CARTESIAN_POINT('',(7.51,4.,2.98));
#12672=CARTESIAN_POINT('',(7.51,4.,2.98));
#12673=CARTESIAN_POINT('',(7.51,4.,3.));
#12674=CARTESIAN_POINT('',(7.51,4.,2.89));
#12675=CARTESIAN_POINT('',(7.51,4.2,3.));
#12676=CARTESIAN_POINT('Origin',(7.49,4.3,2.98));
#12677=CARTESIAN_POINT('',(7.49,4.,2.98));
#12678=CARTESIAN_POINT('',(7.49,4.3,2.98));
#12679=CARTESIAN_POINT('',(7.49,4.,3.));
#12680=CARTESIAN_POINT('',(7.49,4.35,3.));
#12681=CARTESIAN_POINT('',(7.49,4.,2.89));
#12682=CARTESIAN_POINT('Origin',(7.5,4.15,2.98));
#12683=CARTESIAN_POINT('',(4.25,4.,2.98));
#12684=CARTESIAN_POINT('Origin',(8.51,4.3,2.98));
#12685=CARTESIAN_POINT('',(8.51,4.3,2.98));
#12686=CARTESIAN_POINT('',(8.49,4.3,2.98));
#12687=CARTESIAN_POINT('',(8.51,4.3,2.98));
#12688=CARTESIAN_POINT('',(8.51,4.3,3.));
#12689=CARTESIAN_POINT('',(8.51,4.3,2.98));
#12690=CARTESIAN_POINT('',(8.49,4.3,3.));
#12691=CARTESIAN_POINT('',(9.755,4.3,3.));
#12692=CARTESIAN_POINT('',(8.49,4.3,2.98));
#12693=CARTESIAN_POINT('Origin',(8.51,4.,2.98));
#12694=CARTESIAN_POINT('',(8.51,4.,2.98));
#12695=CARTESIAN_POINT('',(8.51,4.,2.98));
#12696=CARTESIAN_POINT('',(8.51,4.,3.));
#12697=CARTESIAN_POINT('',(8.51,4.,2.89));
#12698=CARTESIAN_POINT('',(8.51,4.2,3.));
#12699=CARTESIAN_POINT('Origin',(8.49,4.3,2.98));
#12700=CARTESIAN_POINT('',(8.49,4.,2.98));
#12701=CARTESIAN_POINT('',(8.49,4.3,2.98));
#12702=CARTESIAN_POINT('',(8.49,4.,3.));
#12703=CARTESIAN_POINT('',(8.49,4.35,3.));
#12704=CARTESIAN_POINT('',(8.49,4.,2.89));
#12705=CARTESIAN_POINT('Origin',(8.5,4.15,2.98));
#12706=CARTESIAN_POINT('',(4.75,4.,2.98));
#12707=CARTESIAN_POINT('Origin',(9.51,4.3,2.98));
#12708=CARTESIAN_POINT('',(9.51,4.3,2.98));
#12709=CARTESIAN_POINT('',(9.49,4.3,2.98));
#12710=CARTESIAN_POINT('',(9.51,4.3,2.98));
#12711=CARTESIAN_POINT('',(9.51,4.3,3.));
#12712=CARTESIAN_POINT('',(9.51,4.3,2.98));
#12713=CARTESIAN_POINT('',(9.49,4.3,3.));
#12714=CARTESIAN_POINT('',(10.255,4.3,3.));
#12715=CARTESIAN_POINT('',(9.49,4.3,2.98));
#12716=CARTESIAN_POINT('Origin',(9.51,4.,2.98));
#12717=CARTESIAN_POINT('',(9.51,4.,2.98));
#12718=CARTESIAN_POINT('',(9.51,4.,2.98));
#12719=CARTESIAN_POINT('',(9.51,4.,3.));
#12720=CARTESIAN_POINT('',(9.51,4.,2.89));
#12721=CARTESIAN_POINT('',(9.51,4.2,3.));
#12722=CARTESIAN_POINT('Origin',(9.49,4.3,2.98));
#12723=CARTESIAN_POINT('',(9.49,4.,2.98));
#12724=CARTESIAN_POINT('',(9.49,4.3,2.98));
#12725=CARTESIAN_POINT('',(9.49,4.,3.));
#12726=CARTESIAN_POINT('',(9.49,4.35,3.));
#12727=CARTESIAN_POINT('',(9.49,4.,2.89));
#12728=CARTESIAN_POINT('Origin',(9.5,4.15,2.98));
#12729=CARTESIAN_POINT('',(5.25,4.,2.98));
#12730=CARTESIAN_POINT('Origin',(10.51,4.3,2.98));
#12731=CARTESIAN_POINT('',(10.51,4.3,2.98));
#12732=CARTESIAN_POINT('',(10.49,4.3,2.98));
#12733=CARTESIAN_POINT('',(10.51,4.3,2.98));
#12734=CARTESIAN_POINT('',(10.51,4.3,3.));
#12735=CARTESIAN_POINT('',(10.51,4.3,2.98));
#12736=CARTESIAN_POINT('',(10.49,4.3,3.));
#12737=CARTESIAN_POINT('',(10.755,4.3,3.));
#12738=CARTESIAN_POINT('',(10.49,4.3,2.98));
#12739=CARTESIAN_POINT('Origin',(10.51,4.,2.98));
#12740=CARTESIAN_POINT('',(10.51,4.,2.98));
#12741=CARTESIAN_POINT('',(10.51,4.,2.98));
#12742=CARTESIAN_POINT('',(10.51,4.,3.));
#12743=CARTESIAN_POINT('',(10.51,4.,2.89));
#12744=CARTESIAN_POINT('',(10.51,4.2,3.));
#12745=CARTESIAN_POINT('Origin',(10.49,4.3,2.98));
#12746=CARTESIAN_POINT('',(10.49,4.,2.98));
#12747=CARTESIAN_POINT('',(10.49,4.3,2.98));
#12748=CARTESIAN_POINT('',(10.49,4.,3.));
#12749=CARTESIAN_POINT('',(10.49,4.35,3.));
#12750=CARTESIAN_POINT('',(10.49,4.,2.89));
#12751=CARTESIAN_POINT('Origin',(10.5,4.15,2.98));
#12752=CARTESIAN_POINT('',(5.75,4.,2.98));
#12753=CARTESIAN_POINT('Origin',(4.01,4.5,2.98));
#12754=CARTESIAN_POINT('',(4.01,4.5,2.98));
#12755=CARTESIAN_POINT('',(3.99,4.5,2.98));
#12756=CARTESIAN_POINT('',(4.01,4.5,2.98));
#12757=CARTESIAN_POINT('',(4.01,4.5,3.));
#12758=CARTESIAN_POINT('',(4.01,4.5,2.98));
#12759=CARTESIAN_POINT('',(3.99,4.5,3.));
#12760=CARTESIAN_POINT('',(7.505,4.5,3.));
#12761=CARTESIAN_POINT('',(3.99,4.5,2.98));
#12762=CARTESIAN_POINT('Origin',(4.01,4.,2.98));
#12763=CARTESIAN_POINT('',(4.01,4.,2.98));
#12764=CARTESIAN_POINT('',(4.01,4.,2.98));
#12765=CARTESIAN_POINT('',(4.01,4.,3.));
#12766=CARTESIAN_POINT('',(4.01,4.,2.89));
#12767=CARTESIAN_POINT('',(4.01,4.2,3.));
#12768=CARTESIAN_POINT('Origin',(3.99,4.5,2.98));
#12769=CARTESIAN_POINT('',(3.99,4.,2.98));
#12770=CARTESIAN_POINT('',(3.99,4.5,2.98));
#12771=CARTESIAN_POINT('',(3.99,4.,3.));
#12772=CARTESIAN_POINT('',(3.99,4.45,3.));
#12773=CARTESIAN_POINT('',(3.99,4.,2.89));
#12774=CARTESIAN_POINT('Origin',(4.,4.25,2.98));
#12775=CARTESIAN_POINT('',(2.5,4.,2.98));
#12776=CARTESIAN_POINT('Origin',(12.01,4.5,2.98));
#12777=CARTESIAN_POINT('',(12.01,4.5,2.98));
#12778=CARTESIAN_POINT('',(11.99,4.5,2.98));
#12779=CARTESIAN_POINT('',(12.01,4.5,2.98));
#12780=CARTESIAN_POINT('',(12.01,4.5,3.));
#12781=CARTESIAN_POINT('',(12.01,4.5,2.98));
#12782=CARTESIAN_POINT('',(11.99,4.5,3.));
#12783=CARTESIAN_POINT('',(11.505,4.5,3.));
#12784=CARTESIAN_POINT('',(11.99,4.5,2.98));
#12785=CARTESIAN_POINT('Origin',(12.01,4.,2.98));
#12786=CARTESIAN_POINT('',(12.01,4.,2.98));
#12787=CARTESIAN_POINT('',(12.01,4.,2.98));
#12788=CARTESIAN_POINT('',(12.01,4.,3.));
#12789=CARTESIAN_POINT('',(12.01,4.,2.89));
#12790=CARTESIAN_POINT('',(12.01,4.2,3.));
#12791=CARTESIAN_POINT('Origin',(11.99,4.5,2.98));
#12792=CARTESIAN_POINT('',(11.99,4.,2.98));
#12793=CARTESIAN_POINT('',(11.99,4.5,2.98));
#12794=CARTESIAN_POINT('',(11.99,4.,3.));
#12795=CARTESIAN_POINT('',(11.99,4.45,3.));
#12796=CARTESIAN_POINT('',(11.99,4.,2.89));
#12797=CARTESIAN_POINT('Origin',(12.,4.25,2.98));
#12798=CARTESIAN_POINT('',(6.5,4.,2.98));
#12799=CARTESIAN_POINT('Origin',(13.01,4.5,2.98));
#12800=CARTESIAN_POINT('',(13.01,4.5,2.98));
#12801=CARTESIAN_POINT('',(12.99,4.5,2.98));
#12802=CARTESIAN_POINT('',(13.01,4.5,2.98));
#12803=CARTESIAN_POINT('',(13.01,4.5,3.));
#12804=CARTESIAN_POINT('',(13.01,4.5,2.98));
#12805=CARTESIAN_POINT('',(12.99,4.5,3.));
#12806=CARTESIAN_POINT('',(12.005,4.5,3.));
#12807=CARTESIAN_POINT('',(12.99,4.5,2.98));
#12808=CARTESIAN_POINT('Origin',(13.01,4.,2.98));
#12809=CARTESIAN_POINT('',(13.01,4.,2.98));
#12810=CARTESIAN_POINT('',(13.01,4.,2.98));
#12811=CARTESIAN_POINT('',(13.01,4.,3.));
#12812=CARTESIAN_POINT('',(13.01,4.,2.89));
#12813=CARTESIAN_POINT('',(13.01,4.2,3.));
#12814=CARTESIAN_POINT('Origin',(12.99,4.5,2.98));
#12815=CARTESIAN_POINT('',(12.99,4.,2.98));
#12816=CARTESIAN_POINT('',(12.99,4.5,2.98));
#12817=CARTESIAN_POINT('',(12.99,4.,3.));
#12818=CARTESIAN_POINT('',(12.99,4.45,3.));
#12819=CARTESIAN_POINT('',(12.99,4.,2.89));
#12820=CARTESIAN_POINT('Origin',(13.,4.25,2.98));
#12821=CARTESIAN_POINT('',(7.,4.,2.98));
#12822=CARTESIAN_POINT('Origin',(14.01,4.5,2.98));
#12823=CARTESIAN_POINT('',(14.01,4.5,2.98));
#12824=CARTESIAN_POINT('',(13.99,4.5,2.98));
#12825=CARTESIAN_POINT('',(14.01,4.5,2.98));
#12826=CARTESIAN_POINT('',(14.01,4.5,3.));
#12827=CARTESIAN_POINT('',(14.01,4.5,2.98));
#12828=CARTESIAN_POINT('',(13.99,4.5,3.));
#12829=CARTESIAN_POINT('',(12.505,4.5,3.));
#12830=CARTESIAN_POINT('',(13.99,4.5,2.98));
#12831=CARTESIAN_POINT('Origin',(14.01,4.,2.98));
#12832=CARTESIAN_POINT('',(14.01,4.,2.98));
#12833=CARTESIAN_POINT('',(14.01,4.,2.98));
#12834=CARTESIAN_POINT('',(14.01,4.,3.));
#12835=CARTESIAN_POINT('',(14.01,4.,2.89));
#12836=CARTESIAN_POINT('',(14.01,4.2,3.));
#12837=CARTESIAN_POINT('Origin',(13.99,4.5,2.98));
#12838=CARTESIAN_POINT('',(13.99,4.,2.98));
#12839=CARTESIAN_POINT('',(13.99,4.5,2.98));
#12840=CARTESIAN_POINT('',(13.99,4.,3.));
#12841=CARTESIAN_POINT('',(13.99,4.45,3.));
#12842=CARTESIAN_POINT('',(13.99,4.,2.89));
#12843=CARTESIAN_POINT('Origin',(14.,4.25,2.98));
#12844=CARTESIAN_POINT('',(7.5,4.,2.98));
#12845=CARTESIAN_POINT('Origin',(15.01,4.5,2.98));
#12846=CARTESIAN_POINT('',(15.01,4.5,2.98));
#12847=CARTESIAN_POINT('',(14.99,4.5,2.98));
#12848=CARTESIAN_POINT('',(15.01,4.5,2.98));
#12849=CARTESIAN_POINT('',(15.01,4.5,3.));
#12850=CARTESIAN_POINT('',(15.01,4.5,2.98));
#12851=CARTESIAN_POINT('',(14.99,4.5,3.));
#12852=CARTESIAN_POINT('',(13.005,4.5,3.));
#12853=CARTESIAN_POINT('',(14.99,4.5,2.98));
#12854=CARTESIAN_POINT('Origin',(15.01,4.,2.98));
#12855=CARTESIAN_POINT('',(15.01,4.,2.98));
#12856=CARTESIAN_POINT('',(15.01,4.,2.98));
#12857=CARTESIAN_POINT('',(15.01,4.,3.));
#12858=CARTESIAN_POINT('',(15.01,4.,2.89));
#12859=CARTESIAN_POINT('',(15.01,4.2,3.));
#12860=CARTESIAN_POINT('Origin',(14.99,4.5,2.98));
#12861=CARTESIAN_POINT('',(14.99,4.,2.98));
#12862=CARTESIAN_POINT('',(14.99,4.5,2.98));
#12863=CARTESIAN_POINT('',(14.99,4.,3.));
#12864=CARTESIAN_POINT('',(14.99,4.45,3.));
#12865=CARTESIAN_POINT('',(14.99,4.,2.89));
#12866=CARTESIAN_POINT('Origin',(15.,4.25,2.98));
#12867=CARTESIAN_POINT('',(8.,4.,2.98));
#12868=CARTESIAN_POINT('Origin',(16.01,4.5,2.98));
#12869=CARTESIAN_POINT('',(16.01,4.5,2.98));
#12870=CARTESIAN_POINT('',(15.99,4.5,2.98));
#12871=CARTESIAN_POINT('',(16.01,4.5,2.98));
#12872=CARTESIAN_POINT('',(16.01,4.5,3.));
#12873=CARTESIAN_POINT('',(16.01,4.5,2.98));
#12874=CARTESIAN_POINT('',(15.99,4.5,3.));
#12875=CARTESIAN_POINT('',(13.505,4.5,3.));
#12876=CARTESIAN_POINT('',(15.99,4.5,2.98));
#12877=CARTESIAN_POINT('Origin',(16.01,4.,2.98));
#12878=CARTESIAN_POINT('',(16.01,4.,2.98));
#12879=CARTESIAN_POINT('',(16.01,4.,2.98));
#12880=CARTESIAN_POINT('',(16.01,4.,3.));
#12881=CARTESIAN_POINT('',(16.01,4.,2.89));
#12882=CARTESIAN_POINT('',(16.01,4.2,3.));
#12883=CARTESIAN_POINT('Origin',(15.99,4.5,2.98));
#12884=CARTESIAN_POINT('',(15.99,4.,2.98));
#12885=CARTESIAN_POINT('',(15.99,4.5,2.98));
#12886=CARTESIAN_POINT('',(15.99,4.,3.));
#12887=CARTESIAN_POINT('',(15.99,4.45,3.));
#12888=CARTESIAN_POINT('',(15.99,4.,2.89));
#12889=CARTESIAN_POINT('Origin',(16.,4.25,2.98));
#12890=CARTESIAN_POINT('',(8.5,4.,2.98));
#12891=CARTESIAN_POINT('Origin',(17.01,4.5,2.98));
#12892=CARTESIAN_POINT('',(17.01,4.5,2.98));
#12893=CARTESIAN_POINT('',(16.99,4.5,2.98));
#12894=CARTESIAN_POINT('',(17.01,4.5,2.98));
#12895=CARTESIAN_POINT('',(17.01,4.5,3.));
#12896=CARTESIAN_POINT('',(17.01,4.5,2.98));
#12897=CARTESIAN_POINT('',(16.99,4.5,3.));
#12898=CARTESIAN_POINT('',(14.005,4.5,3.));
#12899=CARTESIAN_POINT('',(16.99,4.5,2.98));
#12900=CARTESIAN_POINT('Origin',(17.01,4.,2.98));
#12901=CARTESIAN_POINT('',(17.01,4.,2.98));
#12902=CARTESIAN_POINT('',(17.01,4.,2.98));
#12903=CARTESIAN_POINT('',(17.01,4.,3.));
#12904=CARTESIAN_POINT('',(17.01,4.,2.89));
#12905=CARTESIAN_POINT('',(17.01,4.2,3.));
#12906=CARTESIAN_POINT('Origin',(16.99,4.5,2.98));
#12907=CARTESIAN_POINT('',(16.99,4.,2.98));
#12908=CARTESIAN_POINT('',(16.99,4.5,2.98));
#12909=CARTESIAN_POINT('',(16.99,4.,3.));
#12910=CARTESIAN_POINT('',(16.99,4.45,3.));
#12911=CARTESIAN_POINT('',(16.99,4.,2.89));
#12912=CARTESIAN_POINT('Origin',(17.,4.25,2.98));
#12913=CARTESIAN_POINT('',(9.,4.,2.98));
#12914=CARTESIAN_POINT('Origin',(18.01,4.5,2.98));
#12915=CARTESIAN_POINT('',(18.01,4.5,2.98));
#12916=CARTESIAN_POINT('',(17.99,4.5,2.98));
#12917=CARTESIAN_POINT('',(18.01,4.5,2.98));
#12918=CARTESIAN_POINT('',(18.01,4.5,3.));
#12919=CARTESIAN_POINT('',(18.01,4.5,2.98));
#12920=CARTESIAN_POINT('',(17.99,4.5,3.));
#12921=CARTESIAN_POINT('',(14.505,4.5,3.));
#12922=CARTESIAN_POINT('',(17.99,4.5,2.98));
#12923=CARTESIAN_POINT('Origin',(18.01,4.,2.98));
#12924=CARTESIAN_POINT('',(18.01,4.,2.98));
#12925=CARTESIAN_POINT('',(18.01,4.,2.98));
#12926=CARTESIAN_POINT('',(18.01,4.,3.));
#12927=CARTESIAN_POINT('',(18.01,4.,2.89));
#12928=CARTESIAN_POINT('',(18.01,4.2,3.));
#12929=CARTESIAN_POINT('Origin',(17.99,4.5,2.98));
#12930=CARTESIAN_POINT('',(17.99,4.,2.98));
#12931=CARTESIAN_POINT('',(17.99,4.5,2.98));
#12932=CARTESIAN_POINT('',(17.99,4.,3.));
#12933=CARTESIAN_POINT('',(17.99,4.45,3.));
#12934=CARTESIAN_POINT('',(17.99,4.,2.89));
#12935=CARTESIAN_POINT('Origin',(18.,4.25,2.98));
#12936=CARTESIAN_POINT('',(9.5,4.,2.98));
#12937=CARTESIAN_POINT('Origin',(11.,4.4,3.));
#12938=CARTESIAN_POINT('',(1.,4.,3.));
#12939=CARTESIAN_POINT('',(21.,4.,3.));
#12940=CARTESIAN_POINT('',(1.,4.,3.));
#12941=CARTESIAN_POINT('',(21.,4.8,3.));
#12942=CARTESIAN_POINT('',(21.,4.,3.));
#12943=CARTESIAN_POINT('',(1.,4.8,3.));
#12944=CARTESIAN_POINT('',(21.,4.8,3.));
#12945=CARTESIAN_POINT('',(1.,4.,3.));
#12946=CARTESIAN_POINT('',(1.,4.8,3.));
#12947=CARTESIAN_POINT('',(1.,4.,3.));
#12948=CARTESIAN_POINT('',(1.,4.,3.));
#12949=CARTESIAN_POINT('',(1.,4.,3.));
#12950=CARTESIAN_POINT('',(1.,4.,3.));
#12951=CARTESIAN_POINT('',(1.,4.,3.));
#12952=CARTESIAN_POINT('',(1.,4.,3.));
#12953=CARTESIAN_POINT('',(1.,4.,3.));
#12954=CARTESIAN_POINT('',(1.,4.,3.));
#12955=CARTESIAN_POINT('',(1.,4.,3.));
#12956=CARTESIAN_POINT('',(1.,4.,3.));
#12957=CARTESIAN_POINT('',(1.,4.,3.));
#12958=CARTESIAN_POINT('',(1.,4.,3.));
#12959=CARTESIAN_POINT('',(1.,4.,3.));
#12960=CARTESIAN_POINT('',(1.,4.,3.));
#12961=CARTESIAN_POINT('',(1.,4.,3.));
#12962=CARTESIAN_POINT('',(1.,4.,3.));
#12963=CARTESIAN_POINT('',(1.,4.,3.));
#12964=CARTESIAN_POINT('',(1.,4.,3.));
#12965=CARTESIAN_POINT('',(1.,4.,3.));
#12966=CARTESIAN_POINT('',(1.,4.,3.));
#12967=CARTESIAN_POINT('',(1.,4.,3.));
#12968=CARTESIAN_POINT('',(1.,4.,3.));
#12969=CARTESIAN_POINT('',(1.,4.,3.));
#12970=CARTESIAN_POINT('',(1.,4.,3.));
#12971=CARTESIAN_POINT('',(1.,4.,3.));
#12972=CARTESIAN_POINT('',(1.,4.,3.));
#12973=CARTESIAN_POINT('',(1.,4.,3.));
#12974=CARTESIAN_POINT('',(1.,4.,3.));
#12975=CARTESIAN_POINT('',(19.775,4.4,3.));
#12976=CARTESIAN_POINT('Origin',(20.,4.4,3.));
#12977=CARTESIAN_POINT('',(1.775,4.4,3.));
#12978=CARTESIAN_POINT('Origin',(2.,4.4,3.));
#12979=CARTESIAN_POINT('Origin',(2.,4.4,2.7));
#12980=CARTESIAN_POINT('',(1.775,4.4,2.8));
#12981=CARTESIAN_POINT('Origin',(2.,4.4,2.8));
#12982=CARTESIAN_POINT('',(1.775,4.4,2.7));
#12983=CARTESIAN_POINT('Origin',(20.,4.4,2.7));
#12984=CARTESIAN_POINT('',(19.775,4.4,2.8));
#12985=CARTESIAN_POINT('Origin',(20.,4.4,2.8));
#12986=CARTESIAN_POINT('',(19.775,4.4,2.7));
#12987=CARTESIAN_POINT('Origin',(21.,4.8,2.8));
#12988=CARTESIAN_POINT('',(21.,4.8,2.8));
#12989=CARTESIAN_POINT('',(1.,4.8,2.8));
#12990=CARTESIAN_POINT('',(21.,4.8,2.8));
#12991=CARTESIAN_POINT('',(1.,4.8,2.8));
#12992=CARTESIAN_POINT('',(21.,4.8,2.8));
#12993=CARTESIAN_POINT('Origin',(21.,4.,2.8));
#12994=CARTESIAN_POINT('',(21.,4.,2.8));
#12995=CARTESIAN_POINT('',(21.,4.,2.8));
#12996=CARTESIAN_POINT('',(21.,4.,2.8));
#12997=CARTESIAN_POINT('Origin',(1.,4.,2.8));
#12998=CARTESIAN_POINT('',(1.,4.,2.8));
#12999=CARTESIAN_POINT('',(1.,4.,2.8));
#13000=CARTESIAN_POINT('',(1.,4.,2.8));
#13001=CARTESIAN_POINT('Origin',(1.,4.8,2.8));
#13002=CARTESIAN_POINT('',(1.,4.8,2.8));
#13003=CARTESIAN_POINT('Origin',(11.,4.4,2.8));
#13004=CARTESIAN_POINT('',(0.,0.,0.));
#13005=CARTESIAN_POINT('Origin',(4.,-2.5,-0.3));
#13006=CARTESIAN_POINT('',(4.,-2.5,-0.3));
#13007=CARTESIAN_POINT('',(2.,-2.5,-0.3));
#13008=CARTESIAN_POINT('',(4.,-2.5,-0.3));
#13009=CARTESIAN_POINT('',(2.,-2.5,0.));
#13010=CARTESIAN_POINT('',(2.,-2.5,-0.3));
#13011=CARTESIAN_POINT('',(4.,-2.5,0.));
#13012=CARTESIAN_POINT('',(4.,-2.5,0.));
#13013=CARTESIAN_POINT('',(4.,-2.5,-0.3));
#13014=CARTESIAN_POINT('Origin',(4.,-4.5,-0.3));
#13015=CARTESIAN_POINT('',(4.,-4.5,-0.3));
#13016=CARTESIAN_POINT('',(4.,-4.5,-0.3));
#13017=CARTESIAN_POINT('',(4.,-4.5,0.));
#13018=CARTESIAN_POINT('',(4.,-4.5,0.));
#13019=CARTESIAN_POINT('',(4.,-4.5,-0.3));
#13020=CARTESIAN_POINT('Origin',(2.,-4.5,-0.3));
#13021=CARTESIAN_POINT('',(2.,-4.5,-0.3));
#13022=CARTESIAN_POINT('',(2.,-4.5,-0.3));
#13023=CARTESIAN_POINT('',(2.,-4.5,0.));
#13024=CARTESIAN_POINT('',(2.,-4.5,0.));
#13025=CARTESIAN_POINT('',(2.,-4.5,-0.3));
#13026=CARTESIAN_POINT('Origin',(2.,-2.5,-0.3));
#13027=CARTESIAN_POINT('',(2.,-2.5,-0.3));
#13028=CARTESIAN_POINT('',(2.,-2.5,0.));
#13029=CARTESIAN_POINT('Origin',(3.,-3.5,0.));
#13030=CARTESIAN_POINT('Origin',(3.,-3.5,-0.3));
#13031=CARTESIAN_POINT('',(0.,0.,0.));
#13032=CARTESIAN_POINT('Origin',(4.,4.5,-0.3));
#13033=CARTESIAN_POINT('',(4.,4.5,-0.3));
#13034=CARTESIAN_POINT('',(2.,4.5,-0.3));
#13035=CARTESIAN_POINT('',(4.,4.5,-0.3));
#13036=CARTESIAN_POINT('',(2.,4.5,0.));
#13037=CARTESIAN_POINT('',(2.,4.5,-0.3));
#13038=CARTESIAN_POINT('',(4.,4.5,0.));
#13039=CARTESIAN_POINT('',(4.,4.5,0.));
#13040=CARTESIAN_POINT('',(4.,4.5,-0.3));
#13041=CARTESIAN_POINT('Origin',(4.,2.5,-0.3));
#13042=CARTESIAN_POINT('',(4.,2.5,-0.3));
#13043=CARTESIAN_POINT('',(4.,2.5,-0.3));
#13044=CARTESIAN_POINT('',(4.,2.5,0.));
#13045=CARTESIAN_POINT('',(4.,2.5,0.));
#13046=CARTESIAN_POINT('',(4.,2.5,-0.3));
#13047=CARTESIAN_POINT('Origin',(2.,2.5,-0.3));
#13048=CARTESIAN_POINT('',(2.,2.5,-0.3));
#13049=CARTESIAN_POINT('',(2.,2.5,-0.3));
#13050=CARTESIAN_POINT('',(2.,2.5,0.));
#13051=CARTESIAN_POINT('',(2.,2.5,0.));
#13052=CARTESIAN_POINT('',(2.,2.5,-0.3));
#13053=CARTESIAN_POINT('Origin',(2.,4.5,-0.3));
#13054=CARTESIAN_POINT('',(2.,4.5,-0.3));
#13055=CARTESIAN_POINT('',(2.,4.5,0.));
#13056=CARTESIAN_POINT('Origin',(3.,3.5,0.));
#13057=CARTESIAN_POINT('Origin',(3.,3.5,-0.3));
#13058=CARTESIAN_POINT('',(0.,0.,0.));
#13059=CARTESIAN_POINT('Origin',(20.,-2.5,-0.3));
#13060=CARTESIAN_POINT('',(20.,-2.5,-0.3));
#13061=CARTESIAN_POINT('',(18.,-2.5,-0.3));
#13062=CARTESIAN_POINT('',(20.,-2.5,-0.3));
#13063=CARTESIAN_POINT('',(18.,-2.5,0.));
#13064=CARTESIAN_POINT('',(18.,-2.5,-0.3));
#13065=CARTESIAN_POINT('',(20.,-2.5,0.));
#13066=CARTESIAN_POINT('',(20.,-2.5,0.));
#13067=CARTESIAN_POINT('',(20.,-2.5,-0.3));
#13068=CARTESIAN_POINT('Origin',(20.,-4.5,-0.3));
#13069=CARTESIAN_POINT('',(20.,-4.5,-0.3));
#13070=CARTESIAN_POINT('',(20.,-4.5,-0.3));
#13071=CARTESIAN_POINT('',(20.,-4.5,0.));
#13072=CARTESIAN_POINT('',(20.,-4.5,0.));
#13073=CARTESIAN_POINT('',(20.,-4.5,-0.3));
#13074=CARTESIAN_POINT('Origin',(18.,-4.5,-0.3));
#13075=CARTESIAN_POINT('',(18.,-4.5,-0.3));
#13076=CARTESIAN_POINT('',(18.,-4.5,-0.3));
#13077=CARTESIAN_POINT('',(18.,-4.5,0.));
#13078=CARTESIAN_POINT('',(18.,-4.5,0.));
#13079=CARTESIAN_POINT('',(18.,-4.5,-0.3));
#13080=CARTESIAN_POINT('Origin',(18.,-2.5,-0.3));
#13081=CARTESIAN_POINT('',(18.,-2.5,-0.3));
#13082=CARTESIAN_POINT('',(18.,-2.5,0.));
#13083=CARTESIAN_POINT('Origin',(19.,-3.5,0.));
#13084=CARTESIAN_POINT('Origin',(19.,-3.5,-0.3));
#13085=CARTESIAN_POINT('',(0.,0.,0.));
#13086=CARTESIAN_POINT('Origin',(20.,4.5,-0.3));
#13087=CARTESIAN_POINT('',(20.,4.5,-0.3));
#13088=CARTESIAN_POINT('',(18.,4.5,-0.3));
#13089=CARTESIAN_POINT('',(20.,4.5,-0.3));
#13090=CARTESIAN_POINT('',(18.,4.5,0.));
#13091=CARTESIAN_POINT('',(18.,4.5,-0.3));
#13092=CARTESIAN_POINT('',(20.,4.5,0.));
#13093=CARTESIAN_POINT('',(20.,4.5,0.));
#13094=CARTESIAN_POINT('',(20.,4.5,-0.3));
#13095=CARTESIAN_POINT('Origin',(20.,2.5,-0.3));
#13096=CARTESIAN_POINT('',(20.,2.5,-0.3));
#13097=CARTESIAN_POINT('',(20.,2.5,-0.3));
#13098=CARTESIAN_POINT('',(20.,2.5,0.));
#13099=CARTESIAN_POINT('',(20.,2.5,0.));
#13100=CARTESIAN_POINT('',(20.,2.5,-0.3));
#13101=CARTESIAN_POINT('Origin',(18.,2.5,-0.3));
#13102=CARTESIAN_POINT('',(18.,2.5,-0.3));
#13103=CARTESIAN_POINT('',(18.,2.5,-0.3));
#13104=CARTESIAN_POINT('',(18.,2.5,0.));
#13105=CARTESIAN_POINT('',(18.,2.5,0.));
#13106=CARTESIAN_POINT('',(18.,2.5,-0.3));
#13107=CARTESIAN_POINT('Origin',(18.,4.5,-0.3));
#13108=CARTESIAN_POINT('',(18.,4.5,-0.3));
#13109=CARTESIAN_POINT('',(18.,4.5,0.));
#13110=CARTESIAN_POINT('Origin',(19.,3.5,0.));
#13111=CARTESIAN_POINT('Origin',(19.,3.5,-0.3));
#13112=CARTESIAN_POINT('',(0.,0.,0.));
#13113=CARTESIAN_POINT('Origin',(14.,0.,0.97));
#13114=CARTESIAN_POINT('',(13.625,-4.59242549680257E-17,0.97));
#13115=CARTESIAN_POINT('Origin',(14.,0.,0.97));
#13116=CARTESIAN_POINT('',(13.625,4.59242549680257E-17,1.5));
#13117=CARTESIAN_POINT('',(13.625,-4.59242549680257E-17,0.97));
#13118=CARTESIAN_POINT('Origin',(14.,0.,1.5));
#13119=CARTESIAN_POINT('Origin',(14.,0.,0.97));
#13120=CARTESIAN_POINT('',(13.775,-2.75545529808154E-17,0.97));
#13121=CARTESIAN_POINT('Origin',(14.,0.,0.97));
#13122=CARTESIAN_POINT('Origin',(8.,0.,0.97));
#13123=CARTESIAN_POINT('',(7.625,-4.59242549680257E-17,0.97));
#13124=CARTESIAN_POINT('Origin',(8.,0.,0.97));
#13125=CARTESIAN_POINT('',(7.625,4.59242549680257E-17,1.5));
#13126=CARTESIAN_POINT('',(7.625,-4.59242549680257E-17,0.97));
#13127=CARTESIAN_POINT('Origin',(8.,0.,1.5));
#13128=CARTESIAN_POINT('Origin',(8.,0.,0.97));
#13129=CARTESIAN_POINT('',(7.775,-2.75545529808154E-17,0.97));
#13130=CARTESIAN_POINT('Origin',(8.,0.,0.97));
#13131=CARTESIAN_POINT('Origin',(2.,0.,0.97));
#13132=CARTESIAN_POINT('',(1.625,-4.59242549680257E-17,0.97));
#13133=CARTESIAN_POINT('Origin',(2.,0.,0.97));
#13134=CARTESIAN_POINT('',(1.625,4.59242549680257E-17,1.5));
#13135=CARTESIAN_POINT('',(1.625,-4.59242549680257E-17,0.97));
#13136=CARTESIAN_POINT('Origin',(2.,0.,1.5));
#13137=CARTESIAN_POINT('Origin',(2.,0.,0.97));
#13138=CARTESIAN_POINT('',(1.775,-2.75545529808155E-17,0.97));
#13139=CARTESIAN_POINT('Origin',(2.,0.,0.97));
#13140=CARTESIAN_POINT('Origin',(20.,0.,0.97));
#13141=CARTESIAN_POINT('',(19.625,-4.59242549680257E-17,0.97));
#13142=CARTESIAN_POINT('Origin',(20.,0.,0.97));
#13143=CARTESIAN_POINT('',(19.625,4.59242549680257E-17,1.5));
#13144=CARTESIAN_POINT('',(19.625,-4.59242549680257E-17,0.97));
#13145=CARTESIAN_POINT('Origin',(20.,0.,1.5));
#13146=CARTESIAN_POINT('Origin',(20.,0.,0.97));
#13147=CARTESIAN_POINT('',(19.775,-2.75545529808156E-17,0.97));
#13148=CARTESIAN_POINT('Origin',(20.,0.,0.97));
#13149=CARTESIAN_POINT('Origin',(14.,0.,-0.1));
#13150=CARTESIAN_POINT('',(13.775,-2.75545529808154E-17,0.));
#13151=CARTESIAN_POINT('Origin',(14.,0.,0.));
#13152=CARTESIAN_POINT('',(13.775,-2.75545529808154E-17,-0.1));
#13153=CARTESIAN_POINT('Origin',(8.,0.,-0.1));
#13154=CARTESIAN_POINT('',(7.775,-2.75545529808154E-17,0.));
#13155=CARTESIAN_POINT('Origin',(8.,0.,0.));
#13156=CARTESIAN_POINT('',(7.775,-2.75545529808154E-17,-0.1));
#13157=CARTESIAN_POINT('Origin',(2.,0.,-0.1));
#13158=CARTESIAN_POINT('',(1.775,-2.75545529808155E-17,0.));
#13159=CARTESIAN_POINT('Origin',(2.,0.,0.));
#13160=CARTESIAN_POINT('',(1.775,-2.75545529808155E-17,-0.1));
#13161=CARTESIAN_POINT('Origin',(20.,0.,-0.1));
#13162=CARTESIAN_POINT('',(19.775,-2.75545529808156E-17,0.));
#13163=CARTESIAN_POINT('Origin',(20.,0.,0.));
#13164=CARTESIAN_POINT('',(19.775,-2.75545529808156E-17,-0.1));
#13165=CARTESIAN_POINT('Origin',(0.,-0.53,1.));
#13166=CARTESIAN_POINT('',(0.,-0.53,1.));
#13167=CARTESIAN_POINT('',(0.,-0.75,0.85));
#13168=CARTESIAN_POINT('',(0.,-0.53,1.));
#13169=CARTESIAN_POINT('',(22.,-0.75,0.85));
#13170=CARTESIAN_POINT('',(0.,-0.75,0.85));
#13171=CARTESIAN_POINT('',(22.,-0.53,1.));
#13172=CARTESIAN_POINT('',(22.,-0.53,1.));
#13173=CARTESIAN_POINT('',(0.,-0.53,1.));
#13174=CARTESIAN_POINT('Origin',(0.,-0.53,1.15));
#13175=CARTESIAN_POINT('',(0.,-0.53,1.15));
#13176=CARTESIAN_POINT('',(0.,-0.53,1.15));
#13177=CARTESIAN_POINT('',(22.,-0.53,1.15));
#13178=CARTESIAN_POINT('',(22.,-0.53,1.15));
#13179=CARTESIAN_POINT('',(0.,-0.53,1.15));
#13180=CARTESIAN_POINT('Origin',(0.,-0.75,1.3));
#13181=CARTESIAN_POINT('',(0.,-0.75,1.3));
#13182=CARTESIAN_POINT('',(0.,-0.75,1.3));
#13183=CARTESIAN_POINT('',(22.,-0.75,1.3));
#13184=CARTESIAN_POINT('',(22.,-0.75,1.3));
#13185=CARTESIAN_POINT('',(0.,-0.75,1.3));
#13186=CARTESIAN_POINT('Origin',(0.,-0.75,1.5));
#13187=CARTESIAN_POINT('',(0.,-0.75,1.5));
#13188=CARTESIAN_POINT('',(0.,-0.75,1.5));
#13189=CARTESIAN_POINT('',(22.,-0.75,1.5));
#13190=CARTESIAN_POINT('',(22.,-0.75,1.5));
#13191=CARTESIAN_POINT('',(0.,-0.75,1.5));
#13192=CARTESIAN_POINT('Origin',(0.,0.75,1.5));
#13193=CARTESIAN_POINT('',(0.,0.75,1.5));
#13194=CARTESIAN_POINT('',(0.,0.75,1.5));
#13195=CARTESIAN_POINT('',(22.,0.75,1.5));
#13196=CARTESIAN_POINT('',(22.,0.75,1.5));
#13197=CARTESIAN_POINT('',(0.,0.75,1.5));
#13198=CARTESIAN_POINT('Origin',(0.,0.75,1.3));
#13199=CARTESIAN_POINT('',(0.,0.75,1.3));
#13200=CARTESIAN_POINT('',(0.,0.75,1.3));
#13201=CARTESIAN_POINT('',(22.,0.75,1.3));
#13202=CARTESIAN_POINT('',(22.,0.75,1.3));
#13203=CARTESIAN_POINT('',(0.,0.75,1.3));
#13204=CARTESIAN_POINT('Origin',(0.,0.53,1.15));
#13205=CARTESIAN_POINT('',(0.,0.53,1.15));
#13206=CARTESIAN_POINT('',(0.,0.53,1.15));
#13207=CARTESIAN_POINT('',(22.,0.53,1.15));
#13208=CARTESIAN_POINT('',(22.,0.53,1.15));
#13209=CARTESIAN_POINT('',(0.,0.53,1.15));
#13210=CARTESIAN_POINT('Origin',(0.,0.53,1.));
#13211=CARTESIAN_POINT('',(0.,0.53,1.));
#13212=CARTESIAN_POINT('',(0.,0.53,1.));
#13213=CARTESIAN_POINT('',(22.,0.53,1.));
#13214=CARTESIAN_POINT('',(22.,0.53,1.));
#13215=CARTESIAN_POINT('',(0.,0.53,1.));
#13216=CARTESIAN_POINT('Origin',(0.,0.75,0.85));
#13217=CARTESIAN_POINT('',(0.,0.75,0.85));
#13218=CARTESIAN_POINT('',(0.,0.75,0.85));
#13219=CARTESIAN_POINT('',(22.,0.75,0.85));
#13220=CARTESIAN_POINT('',(22.,0.75,0.85));
#13221=CARTESIAN_POINT('',(0.,0.75,0.85));
#13222=CARTESIAN_POINT('Origin',(0.,0.75,0.));
#13223=CARTESIAN_POINT('',(0.,0.75,0.));
#13224=CARTESIAN_POINT('',(0.,0.75,0.));
#13225=CARTESIAN_POINT('',(22.,0.75,0.));
#13226=CARTESIAN_POINT('',(22.,0.75,0.));
#13227=CARTESIAN_POINT('',(0.,0.75,0.));
#13228=CARTESIAN_POINT('Origin',(0.,-0.75,0.));
#13229=CARTESIAN_POINT('',(0.,-0.75,0.));
#13230=CARTESIAN_POINT('',(0.,-0.75,0.));
#13231=CARTESIAN_POINT('',(22.,-0.75,0.));
#13232=CARTESIAN_POINT('',(22.,-0.75,0.));
#13233=CARTESIAN_POINT('',(0.,-0.75,0.));
#13234=CARTESIAN_POINT('Origin',(0.,-0.75,0.85));
#13235=CARTESIAN_POINT('',(0.,-0.75,0.85));
#13236=CARTESIAN_POINT('',(22.,-0.75,0.85));
#13237=CARTESIAN_POINT('Origin',(22.,0.,0.75));
#13238=CARTESIAN_POINT('Origin',(0.,0.,0.75));
#13239=CARTESIAN_POINT('',(0.,0.,0.));
#13240=CARTESIAN_POINT('Origin',(-0.1,0.82,-0.3));
#13241=CARTESIAN_POINT('',(0.,0.82,-0.3));
#13242=CARTESIAN_POINT('',(0.,1.,-0.3));
#13243=CARTESIAN_POINT('',(0.,0.41,-0.3));
#13244=CARTESIAN_POINT('',(20.,0.82,-0.3));
#13245=CARTESIAN_POINT('',(-0.1,0.82,-0.3));
#13246=CARTESIAN_POINT('',(20.,1.,-0.3));
#13247=CARTESIAN_POINT('',(20.,0.41,-0.3));
#13248=CARTESIAN_POINT('',(-0.05,1.,-0.3));
#13249=CARTESIAN_POINT('Origin',(-0.1,0.82,-0.55));
#13250=CARTESIAN_POINT('',(0.,0.82,-0.55));
#13251=CARTESIAN_POINT('',(0.,0.82,-0.275));
#13252=CARTESIAN_POINT('',(20.,0.82,-0.55));
#13253=CARTESIAN_POINT('',(-0.1,0.82,-0.55));
#13254=CARTESIAN_POINT('',(20.,0.82,-0.275));
#13255=CARTESIAN_POINT('Origin',(-0.1,0.67,-0.55));
#13256=CARTESIAN_POINT('',(0.,0.67,-0.55));
#13257=CARTESIAN_POINT('',(0.,0.335,-0.55));
#13258=CARTESIAN_POINT('',(20.,0.67,-0.55));
#13259=CARTESIAN_POINT('',(-0.1,0.67,-0.55));
#13260=CARTESIAN_POINT('',(20.,0.335,-0.55));
#13261=CARTESIAN_POINT('Origin',(-0.1,0.42,-0.3));
#13262=CARTESIAN_POINT('',(0.,0.42,-0.3));
#13263=CARTESIAN_POINT('',(0.,0.24,-0.12));
#13264=CARTESIAN_POINT('',(20.,0.42,-0.3));
#13265=CARTESIAN_POINT('',(-0.1,0.42,-0.3));
#13266=CARTESIAN_POINT('',(20.,0.24,-0.12));
#13267=CARTESIAN_POINT('Origin',(-0.1,0.42,0.3));
#13268=CARTESIAN_POINT('',(0.,0.42,0.3));
#13269=CARTESIAN_POINT('',(0.,0.42,0.15));
#13270=CARTESIAN_POINT('',(20.,0.42,0.3));
#13271=CARTESIAN_POINT('',(-0.1,0.42,0.3));
#13272=CARTESIAN_POINT('',(20.,0.42,0.15));
#13273=CARTESIAN_POINT('Origin',(-0.1,0.67,0.55));
#13274=CARTESIAN_POINT('',(0.,0.67,0.55));
#13275=CARTESIAN_POINT('',(6.93889390390723E-18,0.365,0.245));
#13276=CARTESIAN_POINT('',(20.,0.67,0.55));
#13277=CARTESIAN_POINT('',(-0.1,0.67,0.55));
#13278=CARTESIAN_POINT('',(20.,0.365,0.245));
#13279=CARTESIAN_POINT('Origin',(-0.1,0.82,0.55));
#13280=CARTESIAN_POINT('',(0.,0.82,0.55));
#13281=CARTESIAN_POINT('',(0.,0.41,0.55));
#13282=CARTESIAN_POINT('',(20.,0.82,0.55));
#13283=CARTESIAN_POINT('',(-0.1,0.82,0.55));
#13284=CARTESIAN_POINT('',(20.,0.41,0.55));
#13285=CARTESIAN_POINT('Origin',(-0.1,0.82,0.3));
#13286=CARTESIAN_POINT('',(0.,0.82,0.3));
#13287=CARTESIAN_POINT('',(0.,0.82,0.15));
#13288=CARTESIAN_POINT('',(20.,0.82,0.3));
#13289=CARTESIAN_POINT('',(-0.1,0.82,0.3));
#13290=CARTESIAN_POINT('',(20.,0.82,0.15));
#13291=CARTESIAN_POINT('Origin',(-0.1,1.05,0.3));
#13292=CARTESIAN_POINT('',(0.,1.,0.3));
#13293=CARTESIAN_POINT('',(0.,0.525,0.3));
#13294=CARTESIAN_POINT('',(20.,1.,0.3));
#13295=CARTESIAN_POINT('',(-0.05,1.,0.3));
#13296=CARTESIAN_POINT('',(20.,0.525,0.3));
#13297=CARTESIAN_POINT('Origin',(-0.1,-0.3,-0.82));
#13298=CARTESIAN_POINT('',(0.,-0.3,-0.82));
#13299=CARTESIAN_POINT('',(0.,-0.3,-1.));
#13300=CARTESIAN_POINT('',(0.,-0.3,-0.41));
#13301=CARTESIAN_POINT('',(20.,-0.3,-0.82));
#13302=CARTESIAN_POINT('',(-0.1,-0.3,-0.82));
#13303=CARTESIAN_POINT('',(20.,-0.3,-1.));
#13304=CARTESIAN_POINT('',(20.,-0.3,-0.41));
#13305=CARTESIAN_POINT('',(-0.05,-0.3,-1.));
#13306=CARTESIAN_POINT('Origin',(-0.1,-0.55,-0.82));
#13307=CARTESIAN_POINT('',(0.,-0.55,-0.82));
#13308=CARTESIAN_POINT('',(0.,-0.275,-0.82));
#13309=CARTESIAN_POINT('',(20.,-0.55,-0.82));
#13310=CARTESIAN_POINT('',(-0.1,-0.55,-0.82));
#13311=CARTESIAN_POINT('',(20.,-0.275,-0.82));
#13312=CARTESIAN_POINT('Origin',(-0.1,-0.55,-0.67));
#13313=CARTESIAN_POINT('',(0.,-0.55,-0.67));
#13314=CARTESIAN_POINT('',(0.,-0.55,-0.335));
#13315=CARTESIAN_POINT('',(20.,-0.55,-0.67));
#13316=CARTESIAN_POINT('',(-0.1,-0.55,-0.67));
#13317=CARTESIAN_POINT('',(20.,-0.55,-0.335));
#13318=CARTESIAN_POINT('Origin',(-0.1,-0.3,-0.42));
#13319=CARTESIAN_POINT('',(0.,-0.3,-0.42));
#13320=CARTESIAN_POINT('',(0.,-0.12,-0.24));
#13321=CARTESIAN_POINT('',(20.,-0.3,-0.42));
#13322=CARTESIAN_POINT('',(-0.1,-0.3,-0.42));
#13323=CARTESIAN_POINT('',(20.,-0.12,-0.24));
#13324=CARTESIAN_POINT('Origin',(-0.1,0.3,-0.42));
#13325=CARTESIAN_POINT('',(0.,0.3,-0.42));
#13326=CARTESIAN_POINT('',(0.,0.15,-0.42));
#13327=CARTESIAN_POINT('',(20.,0.3,-0.42));
#13328=CARTESIAN_POINT('',(-0.1,0.3,-0.42));
#13329=CARTESIAN_POINT('',(20.,0.15,-0.42));
#13330=CARTESIAN_POINT('Origin',(-0.1,0.55,-0.67));
#13331=CARTESIAN_POINT('',(0.,0.55,-0.67));
#13332=CARTESIAN_POINT('',(0.,0.245,-0.365));
#13333=CARTESIAN_POINT('',(20.,0.55,-0.67));
#13334=CARTESIAN_POINT('',(-0.1,0.55,-0.67));
#13335=CARTESIAN_POINT('',(20.,0.245,-0.365));
#13336=CARTESIAN_POINT('Origin',(-0.1,0.55,-0.82));
#13337=CARTESIAN_POINT('',(0.,0.55,-0.82));
#13338=CARTESIAN_POINT('',(0.,0.55,-0.41));
#13339=CARTESIAN_POINT('',(20.,0.55,-0.82));
#13340=CARTESIAN_POINT('',(-0.1,0.55,-0.82));
#13341=CARTESIAN_POINT('',(20.,0.55,-0.41));
#13342=CARTESIAN_POINT('Origin',(-0.1,0.3,-0.82));
#13343=CARTESIAN_POINT('',(0.,0.3,-0.82));
#13344=CARTESIAN_POINT('',(0.,0.15,-0.82));
#13345=CARTESIAN_POINT('',(20.,0.3,-0.82));
#13346=CARTESIAN_POINT('',(-0.1,0.3,-0.82));
#13347=CARTESIAN_POINT('',(20.,0.15,-0.82));
#13348=CARTESIAN_POINT('Origin',(-0.1,0.3,-1.05));
#13349=CARTESIAN_POINT('',(0.,0.3,-1.));
#13350=CARTESIAN_POINT('',(0.,0.3,-0.525));
#13351=CARTESIAN_POINT('',(20.,0.3,-1.));
#13352=CARTESIAN_POINT('',(-0.05,0.3,-1.));
#13353=CARTESIAN_POINT('',(20.,0.3,-0.525));
#13354=CARTESIAN_POINT('Origin',(-0.1,-0.82,0.3));
#13355=CARTESIAN_POINT('',(0.,-0.82,0.3));
#13356=CARTESIAN_POINT('',(0.,-1.,0.3));
#13357=CARTESIAN_POINT('',(0.,-0.41,0.3));
#13358=CARTESIAN_POINT('',(20.,-0.82,0.3));
#13359=CARTESIAN_POINT('',(-0.1,-0.82,0.3));
#13360=CARTESIAN_POINT('',(20.,-1.,0.3));
#13361=CARTESIAN_POINT('',(20.,-0.41,0.3));
#13362=CARTESIAN_POINT('',(-0.05,-1.,0.3));
#13363=CARTESIAN_POINT('Origin',(-0.1,-0.82,0.55));
#13364=CARTESIAN_POINT('',(0.,-0.82,0.55));
#13365=CARTESIAN_POINT('',(0.,-0.82,0.275));
#13366=CARTESIAN_POINT('',(20.,-0.82,0.55));
#13367=CARTESIAN_POINT('',(-0.1,-0.82,0.55));
#13368=CARTESIAN_POINT('',(20.,-0.82,0.275));
#13369=CARTESIAN_POINT('Origin',(-0.1,-0.67,0.55));
#13370=CARTESIAN_POINT('',(0.,-0.67,0.55));
#13371=CARTESIAN_POINT('',(0.,-0.335,0.55));
#13372=CARTESIAN_POINT('',(20.,-0.67,0.55));
#13373=CARTESIAN_POINT('',(-0.1,-0.67,0.55));
#13374=CARTESIAN_POINT('',(20.,-0.335,0.55));
#13375=CARTESIAN_POINT('Origin',(-0.1,-0.42,0.3));
#13376=CARTESIAN_POINT('',(0.,-0.42,0.3));
#13377=CARTESIAN_POINT('',(-6.93889390390723E-18,-0.24,0.12));
#13378=CARTESIAN_POINT('',(20.,-0.42,0.3));
#13379=CARTESIAN_POINT('',(-0.1,-0.42,0.3));
#13380=CARTESIAN_POINT('',(20.,-0.24,0.12));
#13381=CARTESIAN_POINT('Origin',(-0.1,-0.42,-0.3));
#13382=CARTESIAN_POINT('',(0.,-0.42,-0.3));
#13383=CARTESIAN_POINT('',(0.,-0.42,-0.15));
#13384=CARTESIAN_POINT('',(20.,-0.42,-0.3));
#13385=CARTESIAN_POINT('',(-0.1,-0.42,-0.3));
#13386=CARTESIAN_POINT('',(20.,-0.42,-0.15));
#13387=CARTESIAN_POINT('Origin',(-0.1,-0.67,-0.55));
#13388=CARTESIAN_POINT('',(0.,-0.67,-0.55));
#13389=CARTESIAN_POINT('',(0.,-0.365,-0.245));
#13390=CARTESIAN_POINT('',(20.,-0.67,-0.55));
#13391=CARTESIAN_POINT('',(-0.1,-0.67,-0.55));
#13392=CARTESIAN_POINT('',(20.,-0.365,-0.245));
#13393=CARTESIAN_POINT('Origin',(-0.1,-0.82,-0.55));
#13394=CARTESIAN_POINT('',(0.,-0.82,-0.55));
#13395=CARTESIAN_POINT('',(0.,-0.41,-0.55));
#13396=CARTESIAN_POINT('',(20.,-0.82,-0.55));
#13397=CARTESIAN_POINT('',(-0.1,-0.82,-0.55));
#13398=CARTESIAN_POINT('',(20.,-0.41,-0.55));
#13399=CARTESIAN_POINT('Origin',(-0.1,-0.82,-0.3));
#13400=CARTESIAN_POINT('',(0.,-0.82,-0.3));
#13401=CARTESIAN_POINT('',(0.,-0.82,-0.15));
#13402=CARTESIAN_POINT('',(20.,-0.82,-0.3));
#13403=CARTESIAN_POINT('',(-0.1,-0.82,-0.3));
#13404=CARTESIAN_POINT('',(20.,-0.82,-0.15));
#13405=CARTESIAN_POINT('Origin',(-0.1,-1.05,-0.3));
#13406=CARTESIAN_POINT('',(0.,-1.,-0.3));
#13407=CARTESIAN_POINT('',(0.,-0.525,-0.3));
#13408=CARTESIAN_POINT('',(20.,-1.,-0.3));
#13409=CARTESIAN_POINT('',(-0.05,-1.,-0.3));
#13410=CARTESIAN_POINT('',(20.,-0.525,-0.3));
#13411=CARTESIAN_POINT('Origin',(-0.1,0.3,0.82));
#13412=CARTESIAN_POINT('',(0.,0.3,0.82));
#13413=CARTESIAN_POINT('',(0.,0.3,1.));
#13414=CARTESIAN_POINT('',(0.,0.3,0.41));
#13415=CARTESIAN_POINT('',(20.,0.3,0.82));
#13416=CARTESIAN_POINT('',(-0.1,0.3,0.82));
#13417=CARTESIAN_POINT('',(20.,0.3,1.));
#13418=CARTESIAN_POINT('',(20.,0.3,0.41));
#13419=CARTESIAN_POINT('',(-0.05,0.3,1.));
#13420=CARTESIAN_POINT('Origin',(-0.1,0.55,0.82));
#13421=CARTESIAN_POINT('',(0.,0.55,0.82));
#13422=CARTESIAN_POINT('',(0.,0.275,0.82));
#13423=CARTESIAN_POINT('',(20.,0.55,0.82));
#13424=CARTESIAN_POINT('',(-0.1,0.55,0.82));
#13425=CARTESIAN_POINT('',(20.,0.275,0.82));
#13426=CARTESIAN_POINT('Origin',(-0.1,0.55,0.67));
#13427=CARTESIAN_POINT('',(0.,0.55,0.67));
#13428=CARTESIAN_POINT('',(0.,0.55,0.335));
#13429=CARTESIAN_POINT('',(20.,0.55,0.67));
#13430=CARTESIAN_POINT('',(-0.1,0.55,0.67));
#13431=CARTESIAN_POINT('',(20.,0.55,0.335));
#13432=CARTESIAN_POINT('Origin',(-0.1,0.3,0.42));
#13433=CARTESIAN_POINT('',(0.,0.3,0.42));
#13434=CARTESIAN_POINT('',(6.93889390390723E-18,0.12,0.24));
#13435=CARTESIAN_POINT('',(20.,0.3,0.42));
#13436=CARTESIAN_POINT('',(-0.1,0.3,0.42));
#13437=CARTESIAN_POINT('',(20.,0.12,0.24));
#13438=CARTESIAN_POINT('Origin',(-0.1,-0.3,0.42));
#13439=CARTESIAN_POINT('',(0.,-0.3,0.42));
#13440=CARTESIAN_POINT('',(0.,-0.15,0.42));
#13441=CARTESIAN_POINT('',(20.,-0.3,0.42));
#13442=CARTESIAN_POINT('',(-0.1,-0.3,0.42));
#13443=CARTESIAN_POINT('',(20.,-0.15,0.42));
#13444=CARTESIAN_POINT('Origin',(-0.1,-0.55,0.67));
#13445=CARTESIAN_POINT('',(0.,-0.55,0.67));
#13446=CARTESIAN_POINT('',(6.93889390390723E-18,-0.245,0.365));
#13447=CARTESIAN_POINT('',(20.,-0.55,0.67));
#13448=CARTESIAN_POINT('',(-0.1,-0.55,0.67));
#13449=CARTESIAN_POINT('',(20.,-0.245,0.365));
#13450=CARTESIAN_POINT('Origin',(-0.1,-0.55,0.82));
#13451=CARTESIAN_POINT('',(0.,-0.55,0.82));
#13452=CARTESIAN_POINT('',(0.,-0.55,0.41));
#13453=CARTESIAN_POINT('',(20.,-0.55,0.82));
#13454=CARTESIAN_POINT('',(-0.1,-0.55,0.82));
#13455=CARTESIAN_POINT('',(20.,-0.55,0.41));
#13456=CARTESIAN_POINT('Origin',(-0.1,-0.3,0.82));
#13457=CARTESIAN_POINT('',(0.,-0.3,0.82));
#13458=CARTESIAN_POINT('',(0.,-0.15,0.82));
#13459=CARTESIAN_POINT('',(20.,-0.3,0.82));
#13460=CARTESIAN_POINT('',(-0.1,-0.3,0.82));
#13461=CARTESIAN_POINT('',(20.,-0.15,0.82));
#13462=CARTESIAN_POINT('Origin',(-0.1,-0.3,1.05));
#13463=CARTESIAN_POINT('',(0.,-0.3,1.));
#13464=CARTESIAN_POINT('',(0.,-0.3,0.525));
#13465=CARTESIAN_POINT('',(20.,-0.3,1.));
#13466=CARTESIAN_POINT('',(-0.05,-0.3,1.));
#13467=CARTESIAN_POINT('',(20.,-0.3,0.525));
#13468=CARTESIAN_POINT('Origin',(-0.1,0.,0.));
#13469=CARTESIAN_POINT('',(0.,-2.57175827820944E-17,0.21));
#13470=CARTESIAN_POINT('Origin',(0.,0.,0.));
#13471=CARTESIAN_POINT('',(20.,2.57175827820944E-17,0.21));
#13472=CARTESIAN_POINT('',(-0.1,-2.57175827820944E-17,0.21));
#13473=CARTESIAN_POINT('Origin',(20.,0.,0.));
#13474=CARTESIAN_POINT('Origin',(0.,1.,-1.));
#13475=CARTESIAN_POINT('',(0.,1.,1.));
#13476=CARTESIAN_POINT('',(0.,1.,-1.));
#13477=CARTESIAN_POINT('',(20.,1.,1.));
#13478=CARTESIAN_POINT('',(0.,1.,1.));
#13479=CARTESIAN_POINT('',(20.,1.,-1.));
#13480=CARTESIAN_POINT('Origin',(0.,1.,-1.));
#13481=CARTESIAN_POINT('',(20.,1.,-1.));
#13482=CARTESIAN_POINT('',(20.,1.,-1.));
#13483=CARTESIAN_POINT('',(0.,1.,-1.));
#13484=CARTESIAN_POINT('',(0.,1.,-1.));
#13485=CARTESIAN_POINT('',(0.,1.,-1.));
#13486=CARTESIAN_POINT('Origin',(0.,-1.,-1.));
#13487=CARTESIAN_POINT('',(0.,-1.,-1.));
#13488=CARTESIAN_POINT('',(20.,-1.,-1.));
#13489=CARTESIAN_POINT('Origin',(0.,-1.,-1.));
#13490=CARTESIAN_POINT('',(20.,-1.,-1.));
#13491=CARTESIAN_POINT('',(20.,-1.,-1.));
#13492=CARTESIAN_POINT('',(0.,-1.,-1.));
#13493=CARTESIAN_POINT('',(0.,-1.,-1.));
#13494=CARTESIAN_POINT('',(0.,-1.,-1.));
#13495=CARTESIAN_POINT('Origin',(0.,-1.,1.));
#13496=CARTESIAN_POINT('',(0.,-1.,1.));
#13497=CARTESIAN_POINT('',(20.,-1.,1.));
#13498=CARTESIAN_POINT('Origin',(0.,-1.,1.));
#13499=CARTESIAN_POINT('',(20.,-1.,1.));
#13500=CARTESIAN_POINT('',(20.,-1.,1.));
#13501=CARTESIAN_POINT('',(0.,-1.,1.));
#13502=CARTESIAN_POINT('',(0.,-1.,1.));
#13503=CARTESIAN_POINT('',(0.,-1.,1.));
#13504=CARTESIAN_POINT('Origin',(0.,1.,1.));
#13505=CARTESIAN_POINT('',(0.,1.,1.));
#13506=CARTESIAN_POINT('',(20.,1.,1.));
#13507=CARTESIAN_POINT('Origin',(0.,1.,1.));
#13508=CARTESIAN_POINT('',(20.,1.,1.));
#13509=CARTESIAN_POINT('',(0.,1.,1.));
#13510=CARTESIAN_POINT('Origin',(20.,0.,0.));
#13511=CARTESIAN_POINT('Origin',(0.,0.,0.));
#13512=CARTESIAN_POINT('',(0.,0.,0.));
#13513=CARTESIAN_POINT('Origin',(0.,0.395,0.25));
#13514=CARTESIAN_POINT('',(-0.5,0.3,0.25));
#13515=CARTESIAN_POINT('',(0.5,0.3,0.25));
#13516=CARTESIAN_POINT('',(0.25,0.3,0.25));
#13517=CARTESIAN_POINT('',(-0.5,0.5,0.25));
#13518=CARTESIAN_POINT('',(-0.5,0.5,0.25));
#13519=CARTESIAN_POINT('',(0.5,0.5,0.25));
#13520=CARTESIAN_POINT('',(0.5,0.5,0.25));
#13521=CARTESIAN_POINT('',(0.5,0.29,0.25));
#13522=CARTESIAN_POINT('Origin',(0.5,0.5,0.25));
#13523=CARTESIAN_POINT('',(-0.5,0.5,0.4));
#13524=CARTESIAN_POINT('',(-0.5,0.5,0.25));
#13525=CARTESIAN_POINT('',(0.5,0.5,0.4));
#13526=CARTESIAN_POINT('',(0.5,0.5,0.4));
#13527=CARTESIAN_POINT('',(0.5,0.5,0.25));
#13528=CARTESIAN_POINT('Origin',(0.,0.,0.4));
#13529=CARTESIAN_POINT('',(-0.5,-0.5,0.4));
#13530=CARTESIAN_POINT('',(-0.5,0.5,0.4));
#13531=CARTESIAN_POINT('',(0.5,-0.5,0.4));
#13532=CARTESIAN_POINT('',(-0.5,-0.5,0.4));
#13533=CARTESIAN_POINT('',(0.5,-0.3,0.4));
#13534=CARTESIAN_POINT('',(-0.2117,2.59257727379495E-17,0.4));
#13535=CARTESIAN_POINT('Origin',(0.,0.,0.4));
#13536=CARTESIAN_POINT('Origin',(-0.5,0.3,0.));
#13537=CARTESIAN_POINT('',(-0.5,0.3,0.15));
#13538=CARTESIAN_POINT('',(-0.5,0.3,0.));
#13539=CARTESIAN_POINT('',(-0.5,0.15,0.));
#13540=CARTESIAN_POINT('',(-0.5,0.225,0.075));
#13541=CARTESIAN_POINT('',(-0.5,-0.15,0.));
#13542=CARTESIAN_POINT('',(-0.5,0.3,0.));
#13543=CARTESIAN_POINT('',(-0.5,-0.3,0.15));
#13544=CARTESIAN_POINT('',(-0.5,-0.075,-0.075));
#13545=CARTESIAN_POINT('',(-0.5,-0.3,0.25));
#13546=CARTESIAN_POINT('',(-0.5,-0.3,0.));
#13547=CARTESIAN_POINT('',(-0.5,-0.5,0.25));
#13548=CARTESIAN_POINT('',(-0.5,-0.29,0.25));
#13549=CARTESIAN_POINT('',(-0.5,-0.5,0.25));
#13550=CARTESIAN_POINT('Origin',(-0.5,-0.5,0.25));
#13551=CARTESIAN_POINT('',(0.5,-0.5,0.25));
#13552=CARTESIAN_POINT('',(-0.5,-0.5,0.25));
#13553=CARTESIAN_POINT('',(0.5,-0.5,0.25));
#13554=CARTESIAN_POINT('Origin',(0.,-0.395,0.25));
#13555=CARTESIAN_POINT('',(0.5,-0.3,0.25));
#13556=CARTESIAN_POINT('',(-0.25,-0.3,0.25));
#13557=CARTESIAN_POINT('',(0.5,-0.5,0.25));
#13558=CARTESIAN_POINT('Origin',(0.5,-0.3,0.));
#13559=CARTESIAN_POINT('',(0.5,-0.3,0.15));
#13560=CARTESIAN_POINT('',(0.5,-0.3,0.));
#13561=CARTESIAN_POINT('',(0.5,-0.15,0.));
#13562=CARTESIAN_POINT('',(0.5,-0.225,0.075));
#13563=CARTESIAN_POINT('',(0.5,0.15,0.));
#13564=CARTESIAN_POINT('',(0.5,-0.3,0.));
#13565=CARTESIAN_POINT('',(0.5,0.3,0.15));
#13566=CARTESIAN_POINT('',(0.5,0.075,-0.075));
#13567=CARTESIAN_POINT('',(0.5,0.3,0.));
#13568=CARTESIAN_POINT('Origin',(-0.5,-0.3,0.));
#13569=CARTESIAN_POINT('',(-0.25,-0.3,0.15));
#13570=CARTESIAN_POINT('Origin',(-0.25,-0.225,0.075));
#13571=CARTESIAN_POINT('',(-0.149388386429468,-0.15,0.));
#13572=CARTESIAN_POINT('',(-0.25,-0.15,0.));
#13573=CARTESIAN_POINT('',(0.149388386429468,-0.15,0.));
#13574=CARTESIAN_POINT('Origin',(0.,0.,-0.15));
#13575=CARTESIAN_POINT('',(-0.25,-0.15,0.));
#13576=CARTESIAN_POINT('Origin',(0.,0.,-0.1));
#13577=CARTESIAN_POINT('',(-0.2117,-2.59257727379495E-17,0.));
#13578=CARTESIAN_POINT('Origin',(0.,0.,0.));
#13579=CARTESIAN_POINT('',(-0.2117,-2.59257727379495E-17,-0.1));
#13580=CARTESIAN_POINT('',(-0.149388386429468,0.15,0.));
#13581=CARTESIAN_POINT('Origin',(0.,0.,0.));
#13582=CARTESIAN_POINT('',(0.149388386429468,0.15,0.));
#13583=CARTESIAN_POINT('Origin',(0.,0.,-0.15));
#13584=CARTESIAN_POINT('Origin',(0.,0.,0.));
#13585=CARTESIAN_POINT('Origin',(0.,0.,0.));
#13586=CARTESIAN_POINT('',(0.25,0.15,0.));
#13587=CARTESIAN_POINT('Origin',(0.,0.,0.));
#13588=CARTESIAN_POINT('',(0.25,0.15,0.));
#13589=CARTESIAN_POINT('Origin',(0.25,0.225,0.075));
#13590=CARTESIAN_POINT('',(0.25,0.3,0.15));
#13591=CARTESIAN_POINT('Origin',(0.5,0.3,0.));
#13592=CARTESIAN_POINT('',(0.,0.,0.));
#13593=CARTESIAN_POINT('Origin',(0.115470053837925,-0.5,-0.2));
#13594=CARTESIAN_POINT('',(0.23094010767585,-0.5,0.));
#13595=CARTESIAN_POINT('',(0.115470053837925,-0.5,-0.2));
#13596=CARTESIAN_POINT('',(0.23094010767585,-0.5,0.));
#13597=CARTESIAN_POINT('',(0.115470053837925,-0.8,-0.2));
#13598=CARTESIAN_POINT('',(0.115470053837925,-0.5,-0.2));
#13599=CARTESIAN_POINT('',(0.23094010767585,-0.8,0.));
#13600=CARTESIAN_POINT('',(0.23094010767585,-0.8,0.));
#13601=CARTESIAN_POINT('',(0.23094010767585,-0.5,0.));
#13602=CARTESIAN_POINT('Origin',(-0.115470053837925,-0.5,-0.2));
#13603=CARTESIAN_POINT('',(-0.115470053837925,-0.5,-0.2));
#13604=CARTESIAN_POINT('',(0.115470053837925,-0.5,-0.2));
#13605=CARTESIAN_POINT('',(-0.115470053837925,-0.8,-0.2));
#13606=CARTESIAN_POINT('',(-0.115470053837925,-0.5,-0.2));
#13607=CARTESIAN_POINT('',(0.115470053837925,-0.8,-0.2));
#13608=CARTESIAN_POINT('Origin',(-0.23094010767585,-0.5,-2.77555756156289E-17));
#13609=CARTESIAN_POINT('',(-0.23094010767585,-0.5,-2.82820063659975E-17));
#13610=CARTESIAN_POINT('',(-0.115470053837925,-0.5,-0.2));
#13611=CARTESIAN_POINT('',(-0.23094010767585,-0.8,-2.77555756156289E-17));
#13612=CARTESIAN_POINT('',(-0.23094010767585,-0.5,-2.82820063659975E-17));
#13613=CARTESIAN_POINT('',(-0.115470053837925,-0.8,-0.2));
#13614=CARTESIAN_POINT('Origin',(-0.115470053837925,-0.5,0.2));
#13615=CARTESIAN_POINT('',(-0.115470053837925,-0.5,0.2));
#13616=CARTESIAN_POINT('',(-0.23094010767585,-0.5,-2.82820063659975E-17));
#13617=CARTESIAN_POINT('',(-0.115470053837925,-0.8,0.2));
#13618=CARTESIAN_POINT('',(-0.115470053837925,-0.5,0.2));
#13619=CARTESIAN_POINT('',(-0.23094010767585,-0.8,-2.82820063659975E-17));
#13620=CARTESIAN_POINT('Origin',(0.115470053837925,-0.5,0.2));
#13621=CARTESIAN_POINT('',(0.115470053837925,-0.5,0.2));
#13622=CARTESIAN_POINT('',(-0.115470053837925,-0.5,0.2));
#13623=CARTESIAN_POINT('',(0.115470053837925,-0.8,0.2));
#13624=CARTESIAN_POINT('',(0.115470053837925,-0.5,0.2));
#13625=CARTESIAN_POINT('',(-0.115470053837925,-0.8,0.2));
#13626=CARTESIAN_POINT('Origin',(0.23094010767585,-0.5,0.));
#13627=CARTESIAN_POINT('',(0.115470053837925,-0.5,0.2));
#13628=CARTESIAN_POINT('',(0.115470053837925,-0.8,0.2));
#13629=CARTESIAN_POINT('Origin',(0.,-0.5,0.));
#13630=CARTESIAN_POINT('Origin',(0.,-0.8,0.));
#13631=CARTESIAN_POINT('Origin',(0.,-1.4,0.));
#13632=CARTESIAN_POINT('',(-0.24505,-1.4,3.00099698131059E-17));
#13633=CARTESIAN_POINT('Origin',(0.,-1.4,0.));
#13634=CARTESIAN_POINT('Origin',(0.375,0.5,0.));
#13635=CARTESIAN_POINT('',(-0.375,0.5,-4.59242549680257E-17));
#13636=CARTESIAN_POINT('Origin',(0.,0.5,0.));
#13637=CARTESIAN_POINT('Origin',(0.,0.475,0.));
#13638=CARTESIAN_POINT('',(-0.425,0.45,-5.20474889637625E-17));
#13639=CARTESIAN_POINT('Origin',(0.,0.45,0.));
#13640=CARTESIAN_POINT('',(-0.4,0.475,-4.89858719658941E-17));
#13641=CARTESIAN_POINT('Origin',(0.,0.24,0.));
#13642=CARTESIAN_POINT('',(-0.425,0.0299999999999998,-5.20474889637625E-17));
#13643=CARTESIAN_POINT('Origin',(0.,0.0299999999999998,0.));
#13644=CARTESIAN_POINT('',(-0.425,0.24,-5.20474889637625E-17));
#13645=CARTESIAN_POINT('Origin',(0.,0.0150000000000001,0.));
#13646=CARTESIAN_POINT('',(-0.395,4.85722573273506E-17,-4.83735485663204E-17));
#13647=CARTESIAN_POINT('Origin',(0.,0.,0.));
#13648=CARTESIAN_POINT('',(-0.41,0.0150000000000001,-5.02105187650415E-17));
#13649=CARTESIAN_POINT('Origin',(0.27,0.,0.));
#13650=CARTESIAN_POINT('',(-0.27,0.,-3.30654635769785E-17));
#13651=CARTESIAN_POINT('Origin',(0.,0.,0.));
#13652=CARTESIAN_POINT('Origin',(0.,-0.02,0.));
#13653=CARTESIAN_POINT('',(-0.24505,-0.0498999999999999,3.00099698131059E-17));
#13654=CARTESIAN_POINT('Origin',(0.,-0.0498999999999999,0.));
#13655=CARTESIAN_POINT('',(-0.26,-0.02,-3.18408167778312E-17));
#13656=CARTESIAN_POINT('Origin',(0.,-0.995,0.));
#13657=CARTESIAN_POINT('',(-0.24505,-0.995,-3.00099698131059E-17));
#13658=CARTESIAN_POINT('',(0.,0.,0.));
#13659=CARTESIAN_POINT('Origin',(0.0866025403784439,-0.4,-0.15));
#13660=CARTESIAN_POINT('',(0.173205080756888,-0.4,0.));
#13661=CARTESIAN_POINT('',(0.0866025403784439,-0.4,-0.15));
#13662=CARTESIAN_POINT('',(0.173205080756888,-0.4,0.));
#13663=CARTESIAN_POINT('',(0.0866025403784439,-0.64,-0.15));
#13664=CARTESIAN_POINT('',(0.0866025403784439,-0.4,-0.15));
#13665=CARTESIAN_POINT('',(0.173205080756888,-0.64,0.));
#13666=CARTESIAN_POINT('',(0.173205080756888,-0.64,0.));
#13667=CARTESIAN_POINT('',(0.173205080756888,-0.4,0.));
#13668=CARTESIAN_POINT('Origin',(-0.0866025403784438,-0.4,-0.15));
#13669=CARTESIAN_POINT('',(-0.0866025403784438,-0.4,-0.15));
#13670=CARTESIAN_POINT('',(0.0866025403784439,-0.4,-0.15));
#13671=CARTESIAN_POINT('',(-0.0866025403784438,-0.64,-0.15));
#13672=CARTESIAN_POINT('',(-0.0866025403784438,-0.4,-0.15));
#13673=CARTESIAN_POINT('',(0.0866025403784439,-0.64,-0.15));
#13674=CARTESIAN_POINT('Origin',(-0.173205080756888,-0.4,-2.77555756156289E-17));
#13675=CARTESIAN_POINT('',(-0.173205080756888,-0.4,-2.12115047744981E-17));
#13676=CARTESIAN_POINT('',(-0.0866025403784438,-0.4,-0.15));
#13677=CARTESIAN_POINT('',(-0.173205080756888,-0.64,-2.77555756156289E-17));
#13678=CARTESIAN_POINT('',(-0.173205080756888,-0.4,-2.12115047744981E-17));
#13679=CARTESIAN_POINT('',(-0.0866025403784438,-0.64,-0.15));
#13680=CARTESIAN_POINT('Origin',(-0.0866025403784439,-0.4,0.15));
#13681=CARTESIAN_POINT('',(-0.0866025403784439,-0.4,0.15));
#13682=CARTESIAN_POINT('',(-0.173205080756888,-0.4,-2.12115047744981E-17));
#13683=CARTESIAN_POINT('',(-0.0866025403784439,-0.64,0.15));
#13684=CARTESIAN_POINT('',(-0.0866025403784439,-0.4,0.15));
#13685=CARTESIAN_POINT('',(-0.173205080756888,-0.64,-2.12115047744981E-17));
#13686=CARTESIAN_POINT('Origin',(0.0866025403784439,-0.4,0.15));
#13687=CARTESIAN_POINT('',(0.0866025403784439,-0.4,0.15));
#13688=CARTESIAN_POINT('',(-0.0866025403784439,-0.4,0.15));
#13689=CARTESIAN_POINT('',(0.0866025403784439,-0.64,0.15));
#13690=CARTESIAN_POINT('',(0.0866025403784439,-0.4,0.15));
#13691=CARTESIAN_POINT('',(-0.0866025403784439,-0.64,0.15));
#13692=CARTESIAN_POINT('Origin',(0.173205080756888,-0.4,0.));
#13693=CARTESIAN_POINT('',(0.0866025403784439,-0.4,0.15));
#13694=CARTESIAN_POINT('',(0.0866025403784439,-0.64,0.15));
#13695=CARTESIAN_POINT('Origin',(0.,-0.4,-2.77555756156289E-17));
#13696=CARTESIAN_POINT('Origin',(0.,-0.64,-2.77555756156289E-17));
#13697=CARTESIAN_POINT('Origin',(0.,-1.,0.));
#13698=CARTESIAN_POINT('',(-0.1954,-1.,2.39295984553393E-17));
#13699=CARTESIAN_POINT('Origin',(0.,-1.,0.));
#13700=CARTESIAN_POINT('Origin',(0.3,0.4,0.));
#13701=CARTESIAN_POINT('',(-0.3,0.4,-3.67394039744206E-17));
#13702=CARTESIAN_POINT('Origin',(0.,0.4,0.));
#13703=CARTESIAN_POINT('Origin',(0.,0.375,0.));
#13704=CARTESIAN_POINT('',(-0.35,0.35,-4.28626379701573E-17));
#13705=CARTESIAN_POINT('Origin',(0.,0.35,0.));
#13706=CARTESIAN_POINT('',(-0.325,0.375,-3.9801020972289E-17));
#13707=CARTESIAN_POINT('Origin',(0.,0.19,0.));
#13708=CARTESIAN_POINT('',(-0.35,0.03,-4.28626379701574E-17));
#13709=CARTESIAN_POINT('Origin',(0.,0.03,0.));
#13710=CARTESIAN_POINT('',(-0.35,0.19,-4.28626379701574E-17));
#13711=CARTESIAN_POINT('Origin',(0.,0.0149999999999999,0.));
#13712=CARTESIAN_POINT('',(-0.32,-3.29597460435593E-17,-3.91886975727153E-17));
#13713=CARTESIAN_POINT('Origin',(0.,0.,0.));
#13714=CARTESIAN_POINT('',(-0.335,0.0149999999999999,-4.10256677714363E-17));
#13715=CARTESIAN_POINT('Origin',(0.22,0.,0.));
#13716=CARTESIAN_POINT('',(-0.22,-6.93889390390723E-18,-2.69422295812418E-17));
#13717=CARTESIAN_POINT('Origin',(0.,0.,0.));
#13718=CARTESIAN_POINT('Origin',(0.,-0.02,0.));
#13719=CARTESIAN_POINT('',(-0.1954,-0.0492,2.39295984553393E-17));
#13720=CARTESIAN_POINT('Origin',(0.,-0.0492,0.));
#13721=CARTESIAN_POINT('',(-0.21,-0.02,-2.57175827820944E-17));
#13722=CARTESIAN_POINT('Origin',(0.,-0.8,0.));
#13723=CARTESIAN_POINT('',(-0.1954,-0.8,-2.39295984553393E-17));
#13724=CARTESIAN_POINT('',(0.,0.,0.));
#13725=CARTESIAN_POINT('',(0.,0.,0.));
#13726=CARTESIAN_POINT('Origin',(11.,3.5,5.1));
#13727=CARTESIAN_POINT('',(10.835,3.5,5.2));
#13728=CARTESIAN_POINT('Origin',(11.,3.5,5.2));
#13729=CARTESIAN_POINT('',(10.835,3.5,6.4));
#13730=CARTESIAN_POINT('',(10.835,3.5,5.1));
#13731=CARTESIAN_POINT('Origin',(11.,3.5,6.4));
#13732=CARTESIAN_POINT('Origin',(11.,0.,5.1));
#13733=CARTESIAN_POINT('',(10.75,-3.06161699786838E-17,5.2));
#13734=CARTESIAN_POINT('Origin',(11.,0.,5.2));
#13735=CARTESIAN_POINT('',(10.75,3.06161699786838E-17,6.4));
#13736=CARTESIAN_POINT('',(10.75,-3.06161699786838E-17,5.1));
#13737=CARTESIAN_POINT('Origin',(11.,0.,6.4));
#13738=CARTESIAN_POINT('Origin',(12.5,-1.9,5.1));
#13739=CARTESIAN_POINT('',(12.225,-1.9,5.2));
#13740=CARTESIAN_POINT('Origin',(12.5,-1.9,5.2));
#13741=CARTESIAN_POINT('',(12.225,-1.9,6.4));
#13742=CARTESIAN_POINT('',(12.225,-1.9,5.1));
#13743=CARTESIAN_POINT('Origin',(12.5,-1.9,6.4));
#13744=CARTESIAN_POINT('Origin',(9.5,1.9,5.1));
#13745=CARTESIAN_POINT('',(9.225,1.9,5.2));
#13746=CARTESIAN_POINT('Origin',(9.5,1.9,5.2));
#13747=CARTESIAN_POINT('',(9.225,1.9,6.4));
#13748=CARTESIAN_POINT('',(9.225,1.9,5.1));
#13749=CARTESIAN_POINT('Origin',(9.5,1.9,6.4));
#13750=CARTESIAN_POINT('Origin',(9.5,-1.9,5.1));
#13751=CARTESIAN_POINT('',(9.225,-1.9,5.2));
#13752=CARTESIAN_POINT('Origin',(9.5,-1.9,5.2));
#13753=CARTESIAN_POINT('',(9.225,-1.9,6.4));
#13754=CARTESIAN_POINT('',(9.225,-1.9,5.1));
#13755=CARTESIAN_POINT('Origin',(9.5,-1.9,6.4));
#13756=CARTESIAN_POINT('Origin',(12.5,1.9,5.1));
#13757=CARTESIAN_POINT('',(12.225,1.9,5.2));
#13758=CARTESIAN_POINT('Origin',(12.5,1.9,5.2));
#13759=CARTESIAN_POINT('',(12.225,1.9,6.4));
#13760=CARTESIAN_POINT('',(12.225,1.9,5.1));
#13761=CARTESIAN_POINT('Origin',(12.5,1.9,6.4));
#13762=CARTESIAN_POINT('Origin',(15.,4.,5.2));
#13763=CARTESIAN_POINT('',(15.,4.,5.2));
#13764=CARTESIAN_POINT('',(7.,4.,5.2));
#13765=CARTESIAN_POINT('',(15.,4.,5.2));
#13766=CARTESIAN_POINT('',(7.,4.,6.4));
#13767=CARTESIAN_POINT('',(7.,4.,5.2));
#13768=CARTESIAN_POINT('',(15.,4.,6.4));
#13769=CARTESIAN_POINT('',(15.,4.,6.4));
#13770=CARTESIAN_POINT('',(15.,4.,5.2));
#13771=CARTESIAN_POINT('Origin',(15.,-4.,5.2));
#13772=CARTESIAN_POINT('',(15.,-4.,5.2));
#13773=CARTESIAN_POINT('',(15.,-4.,5.2));
#13774=CARTESIAN_POINT('',(15.,-4.,6.4));
#13775=CARTESIAN_POINT('',(15.,-4.,6.4));
#13776=CARTESIAN_POINT('',(15.,-4.,5.2));
#13777=CARTESIAN_POINT('Origin',(7.,-4.,5.2));
#13778=CARTESIAN_POINT('',(7.,-4.,5.2));
#13779=CARTESIAN_POINT('',(7.,-4.,5.2));
#13780=CARTESIAN_POINT('',(7.,-4.,6.4));
#13781=CARTESIAN_POINT('',(7.,-4.,6.4));
#13782=CARTESIAN_POINT('',(7.,-4.,5.2));
#13783=CARTESIAN_POINT('Origin',(7.,4.,5.2));
#13784=CARTESIAN_POINT('',(7.,4.,5.2));
#13785=CARTESIAN_POINT('',(7.,4.,6.4));
#13786=CARTESIAN_POINT('Origin',(11.,0.,6.4));
#13787=CARTESIAN_POINT('Origin',(11.,0.,5.2));
#13788=CARTESIAN_POINT('',(0.,0.,0.));
#13789=CARTESIAN_POINT('Origin',(11.,3.5,6.3));
#13790=CARTESIAN_POINT('',(10.775,3.5,6.4));
#13791=CARTESIAN_POINT('Origin',(11.,3.5,6.4));
#13792=CARTESIAN_POINT('',(10.775,3.5,6.6));
#13793=CARTESIAN_POINT('',(10.775,3.5,6.3));
#13794=CARTESIAN_POINT('Origin',(11.,3.5,6.6));
#13795=CARTESIAN_POINT('Origin',(10.6,4.4,6.6));
#13796=CARTESIAN_POINT('',(10.6,4.4,6.6));
#13797=CARTESIAN_POINT('',(10.6,3.,6.6));
#13798=CARTESIAN_POINT('',(10.6,4.4,6.6));
#13799=CARTESIAN_POINT('',(11.4,3.,6.6));
#13800=CARTESIAN_POINT('',(10.6,3.,6.6));
#13801=CARTESIAN_POINT('',(11.4,4.4,6.6));
#13802=CARTESIAN_POINT('',(11.4,4.4,6.6));
#13803=CARTESIAN_POINT('',(10.6,4.4,6.6));
#13804=CARTESIAN_POINT('Origin',(10.6,4.4,3.1));
#13805=CARTESIAN_POINT('',(10.6,4.4,3.1));
#13806=CARTESIAN_POINT('',(10.6,4.4,3.1));
#13807=CARTESIAN_POINT('',(11.4,4.4,3.1));
#13808=CARTESIAN_POINT('',(11.4,4.4,3.1));
#13809=CARTESIAN_POINT('',(10.6,4.4,3.1));
#13810=CARTESIAN_POINT('Origin',(10.6,4.2,3.1));
#13811=CARTESIAN_POINT('',(10.6,4.2,3.1));
#13812=CARTESIAN_POINT('',(10.6,4.2,3.1));
#13813=CARTESIAN_POINT('',(11.4,4.2,3.1));
#13814=CARTESIAN_POINT('',(11.4,4.2,3.1));
#13815=CARTESIAN_POINT('',(10.6,4.2,3.1));
#13816=CARTESIAN_POINT('Origin',(10.6,4.2,6.4));
#13817=CARTESIAN_POINT('',(10.6,4.2,6.4));
#13818=CARTESIAN_POINT('',(10.6,4.2,6.4));
#13819=CARTESIAN_POINT('',(11.4,4.2,6.4));
#13820=CARTESIAN_POINT('',(11.4,4.2,6.4));
#13821=CARTESIAN_POINT('',(10.6,4.2,6.4));
#13822=CARTESIAN_POINT('Origin',(10.6,3.,6.4));
#13823=CARTESIAN_POINT('',(10.6,3.,6.4));
#13824=CARTESIAN_POINT('',(10.6,3.,6.4));
#13825=CARTESIAN_POINT('',(11.4,3.,6.4));
#13826=CARTESIAN_POINT('',(11.4,3.,6.4));
#13827=CARTESIAN_POINT('',(10.6,3.,6.4));
#13828=CARTESIAN_POINT('Origin',(10.6,3.,6.6));
#13829=CARTESIAN_POINT('',(10.6,3.,6.6));
#13830=CARTESIAN_POINT('',(11.4,3.,6.6));
#13831=CARTESIAN_POINT('Origin',(11.4,3.7,4.85));
#13832=CARTESIAN_POINT('Origin',(10.6,3.7,4.85));
#13833=CARTESIAN_POINT('',(0.,0.,0.));
#13834=CARTESIAN_POINT('Origin',(11.,0.,6.4));
#13835=CARTESIAN_POINT('',(10.67,-4.04133443718627E-17,8.4));
#13836=CARTESIAN_POINT('Origin',(11.,0.,8.4));
#13837=CARTESIAN_POINT('',(10.67,-4.04133443718627E-17,6.4));
#13838=CARTESIAN_POINT('',(10.67,-4.04133443718627E-17,6.4));
#13839=CARTESIAN_POINT('Origin',(11.,0.,6.4));
#13840=CARTESIAN_POINT('Origin',(11.,0.,6.4));
#13841=CARTESIAN_POINT('',(9.5,-1.83697019872103E-16,8.4));
#13842=CARTESIAN_POINT('Origin',(11.,0.,8.4));
#13843=CARTESIAN_POINT('',(9.5,-1.83697019872103E-16,6.4));
#13844=CARTESIAN_POINT('',(9.5,-1.83697019872103E-16,6.4));
#13845=CARTESIAN_POINT('Origin',(11.,0.,6.4));
#13846=CARTESIAN_POINT('Origin',(11.,0.,8.4));
#13847=CARTESIAN_POINT('Origin',(11.,0.,6.4));
#13848=CARTESIAN_POINT('',(0.,0.,0.));
#13849=CARTESIAN_POINT('',(0.,0.,0.));
#13850=CARTESIAN_POINT('Origin',(1.5,-1.9,1.7));
#13851=CARTESIAN_POINT('',(1.56403124237433,-1.7,1.7));
#13852=CARTESIAN_POINT('',(1.43596875762567,-1.7,1.7));
#13853=CARTESIAN_POINT('',(0.75,-1.7,1.7));
#13854=CARTESIAN_POINT('Origin',(1.5,-1.9,1.7));
#13855=CARTESIAN_POINT('Origin',(1.5,-1.9,1.7));
#13856=CARTESIAN_POINT('',(1.56403124237433,-1.7,1.75));
#13857=CARTESIAN_POINT('',(1.56403124237433,-1.7,1.7));
#13858=CARTESIAN_POINT('',(1.29,-1.9,1.75));
#13859=CARTESIAN_POINT('Origin',(1.5,-1.9,1.75));
#13860=CARTESIAN_POINT('',(1.29,-1.9,2.4));
#13861=CARTESIAN_POINT('',(1.29,-1.9,1.7));
#13862=CARTESIAN_POINT('Origin',(1.5,-1.9,2.4));
#13863=CARTESIAN_POINT('',(1.43596875762567,-1.7,1.75));
#13864=CARTESIAN_POINT('Origin',(1.5,-1.9,1.75));
#13865=CARTESIAN_POINT('',(1.43596875762567,-1.7,1.7));
#13866=CARTESIAN_POINT('Origin',(-1.5,1.9,1.7));
#13867=CARTESIAN_POINT('',(-1.56403124237433,1.7,1.7));
#13868=CARTESIAN_POINT('',(-1.43596875762567,1.7,1.7));
#13869=CARTESIAN_POINT('',(-0.75,1.7,1.7));
#13870=CARTESIAN_POINT('Origin',(-1.5,1.9,1.7));
#13871=CARTESIAN_POINT('Origin',(-1.5,1.9,1.7));
#13872=CARTESIAN_POINT('',(-1.56403124237433,1.7,1.75));
#13873=CARTESIAN_POINT('',(-1.56403124237433,1.7,1.7));
#13874=CARTESIAN_POINT('',(-1.71,1.9,1.75));
#13875=CARTESIAN_POINT('Origin',(-1.5,1.9,1.75));
#13876=CARTESIAN_POINT('',(-1.71,1.9,2.4));
#13877=CARTESIAN_POINT('',(-1.71,1.9,1.7));
#13878=CARTESIAN_POINT('Origin',(-1.5,1.9,2.4));
#13879=CARTESIAN_POINT('',(-1.43596875762567,1.7,1.75));
#13880=CARTESIAN_POINT('Origin',(-1.5,1.9,1.75));
#13881=CARTESIAN_POINT('',(-1.43596875762567,1.7,1.7));
#13882=CARTESIAN_POINT('Origin',(-1.5,-1.9,1.7));
#13883=CARTESIAN_POINT('',(-1.43596875762567,-1.7,1.7));
#13884=CARTESIAN_POINT('',(-1.56403124237433,-1.7,1.7));
#13885=CARTESIAN_POINT('',(-0.75,-1.7,1.7));
#13886=CARTESIAN_POINT('Origin',(-1.5,-1.9,1.7));
#13887=CARTESIAN_POINT('Origin',(-1.5,-1.9,1.7));
#13888=CARTESIAN_POINT('',(-1.43596875762567,-1.7,1.75));
#13889=CARTESIAN_POINT('',(-1.43596875762567,-1.7,1.7));
#13890=CARTESIAN_POINT('',(-1.71,-1.9,1.75));
#13891=CARTESIAN_POINT('Origin',(-1.5,-1.9,1.75));
#13892=CARTESIAN_POINT('',(-1.71,-1.9,2.4));
#13893=CARTESIAN_POINT('',(-1.71,-1.9,1.7));
#13894=CARTESIAN_POINT('Origin',(-1.5,-1.9,2.4));
#13895=CARTESIAN_POINT('',(-1.56403124237433,-1.7,1.75));
#13896=CARTESIAN_POINT('Origin',(-1.5,-1.9,1.75));
#13897=CARTESIAN_POINT('',(-1.56403124237433,-1.7,1.7));
#13898=CARTESIAN_POINT('Origin',(1.5,1.9,1.7));
#13899=CARTESIAN_POINT('',(1.43596875762567,1.7,1.7));
#13900=CARTESIAN_POINT('',(1.56403124237433,1.7,1.7));
#13901=CARTESIAN_POINT('',(0.75,1.7,1.7));
#13902=CARTESIAN_POINT('Origin',(1.5,1.9,1.7));
#13903=CARTESIAN_POINT('Origin',(1.5,1.9,1.7));
#13904=CARTESIAN_POINT('',(1.43596875762567,1.7,1.75));
#13905=CARTESIAN_POINT('',(1.43596875762567,1.7,1.7));
#13906=CARTESIAN_POINT('',(1.29,1.9,1.75));
#13907=CARTESIAN_POINT('Origin',(1.5,1.9,1.75));
#13908=CARTESIAN_POINT('',(1.29,1.9,2.4));
#13909=CARTESIAN_POINT('',(1.29,1.9,1.7));
#13910=CARTESIAN_POINT('Origin',(1.5,1.9,2.4));
#13911=CARTESIAN_POINT('',(1.56403124237433,1.7,1.75));
#13912=CARTESIAN_POINT('Origin',(1.5,1.9,1.75));
#13913=CARTESIAN_POINT('',(1.56403124237433,1.7,1.7));
#13914=CARTESIAN_POINT('Origin',(0.,-1.7,1.75));
#13915=CARTESIAN_POINT('',(0.,-1.7,1.75));
#13916=CARTESIAN_POINT('',(-1.97,-1.7,1.75));
#13917=CARTESIAN_POINT('',(0.,-1.7,1.75));
#13918=CARTESIAN_POINT('',(-1.97,-1.7,0.43));
#13919=CARTESIAN_POINT('',(-1.97,-1.7,1.75));
#13920=CARTESIAN_POINT('',(1.97,-1.7,0.43));
#13921=CARTESIAN_POINT('',(0.,-1.7,0.43));
#13922=CARTESIAN_POINT('',(1.97,-1.7,1.75));
#13923=CARTESIAN_POINT('',(1.97,-1.7,1.75));
#13924=CARTESIAN_POINT('',(0.,-1.7,1.75));
#13925=CARTESIAN_POINT('Origin',(0.,1.7,0.43));
#13926=CARTESIAN_POINT('',(0.,1.7,1.75));
#13927=CARTESIAN_POINT('',(1.97,1.7,1.75));
#13928=CARTESIAN_POINT('',(0.,1.7,1.75));
#13929=CARTESIAN_POINT('',(1.97,1.7,0.43));
#13930=CARTESIAN_POINT('',(1.97,1.7,0.43));
#13931=CARTESIAN_POINT('',(-1.97,1.7,0.43));
#13932=CARTESIAN_POINT('',(0.,1.7,0.43));
#13933=CARTESIAN_POINT('',(-1.97,1.7,1.75));
#13934=CARTESIAN_POINT('',(-1.97,1.7,0.43));
#13935=CARTESIAN_POINT('',(0.,1.7,1.75));
#13936=CARTESIAN_POINT('Origin',(-1.97,0.,1.415));
#13937=CARTESIAN_POINT('',(-1.97,-2.35,1.75));
#13938=CARTESIAN_POINT('',(-1.97,-2.35,1.75));
#13939=CARTESIAN_POINT('',(-1.97,-2.35,2.4));
#13940=CARTESIAN_POINT('',(-1.97,-2.35,2.4));
#13941=CARTESIAN_POINT('',(-1.97,2.35,2.4));
#13942=CARTESIAN_POINT('',(-1.97,2.35,2.4));
#13943=CARTESIAN_POINT('',(-1.97,2.35,1.75));
#13944=CARTESIAN_POINT('',(-1.97,2.35,1.75));
#13945=CARTESIAN_POINT('',(-1.97,1.7,1.75));
#13946=CARTESIAN_POINT('',(-1.97,0.78,0.43));
#13947=CARTESIAN_POINT('',(-1.97,0.78,0.43));
#13948=CARTESIAN_POINT('',(-1.97,0.78,1.55));
#13949=CARTESIAN_POINT('',(-1.97,0.78,1.55));
#13950=CARTESIAN_POINT('',(-1.97,-0.78,1.55));
#13951=CARTESIAN_POINT('',(-1.97,-0.78,1.55));
#13952=CARTESIAN_POINT('',(-1.97,-0.78,0.43));
#13953=CARTESIAN_POINT('',(-1.97,-0.78,0.43));
#13954=CARTESIAN_POINT('',(-1.97,-1.7,0.43));
#13955=CARTESIAN_POINT('Origin',(0.,-2.35,1.75));
#13956=CARTESIAN_POINT('',(1.97,-2.35,1.75));
#13957=CARTESIAN_POINT('',(1.97,-2.35,1.75));
#13958=CARTESIAN_POINT('',(0.,-2.35,1.75));
#13959=CARTESIAN_POINT('Origin',(0.,-2.35,2.4));
#13960=CARTESIAN_POINT('',(1.97,-2.35,2.4));
#13961=CARTESIAN_POINT('',(1.97,-2.35,2.4));
#13962=CARTESIAN_POINT('',(0.,-2.35,2.4));
#13963=CARTESIAN_POINT('Origin',(0.,2.35,2.4));
#13964=CARTESIAN_POINT('',(1.97,2.35,2.4));
#13965=CARTESIAN_POINT('',(1.97,2.35,2.4));
#13966=CARTESIAN_POINT('',(0.,2.35,2.4));
#13967=CARTESIAN_POINT('Origin',(0.,2.35,1.75));
#13968=CARTESIAN_POINT('',(1.97,2.35,1.75));
#13969=CARTESIAN_POINT('',(1.97,2.35,1.75));
#13970=CARTESIAN_POINT('',(0.,2.35,1.75));
#13971=CARTESIAN_POINT('Origin',(0.,1.7,1.75));
#13972=CARTESIAN_POINT('',(1.97,1.7,1.75));
#13973=CARTESIAN_POINT('Origin',(0.,0.78,0.43));
#13974=CARTESIAN_POINT('',(1.97,0.78,0.43));
#13975=CARTESIAN_POINT('',(1.97,0.78,0.43));
#13976=CARTESIAN_POINT('',(0.,0.78,0.43));
#13977=CARTESIAN_POINT('Origin',(0.,0.78,1.55));
#13978=CARTESIAN_POINT('',(1.97,0.78,1.55));
#13979=CARTESIAN_POINT('',(1.97,0.78,1.55));
#13980=CARTESIAN_POINT('',(0.,0.78,1.55));
#13981=CARTESIAN_POINT('Origin',(0.,-0.78,1.55));
#13982=CARTESIAN_POINT('',(1.97,-0.78,1.55));
#13983=CARTESIAN_POINT('',(1.97,-0.78,1.55));
#13984=CARTESIAN_POINT('',(0.,-0.78,1.55));
#13985=CARTESIAN_POINT('Origin',(0.,-0.78,0.43));
#13986=CARTESIAN_POINT('',(1.97,-0.78,0.43));
#13987=CARTESIAN_POINT('',(1.97,-0.78,0.43));
#13988=CARTESIAN_POINT('',(0.,-0.78,0.43));
#13989=CARTESIAN_POINT('Origin',(0.,-1.7,0.43));
#13990=CARTESIAN_POINT('',(1.97,-1.7,0.43));
#13991=CARTESIAN_POINT('Origin',(1.97,0.,1.415));
#13992=CARTESIAN_POINT('',(0.,0.,0.));
#13993=CARTESIAN_POINT('Origin',(1.97,1.7,2.3));
#13994=CARTESIAN_POINT('',(1.97,1.7,2.3));
#13995=CARTESIAN_POINT('',(1.97,-1.7,2.3));
#13996=CARTESIAN_POINT('',(1.97,1.7,2.3));
#13997=CARTESIAN_POINT('',(3.07,-1.7,2.3));
#13998=CARTESIAN_POINT('',(1.97,-1.7,2.3));
#13999=CARTESIAN_POINT('',(3.07,1.7,2.3));
#14000=CARTESIAN_POINT('',(3.07,1.7,2.3));
#14001=CARTESIAN_POINT('',(1.97,1.7,2.3));
#14002=CARTESIAN_POINT('Origin',(1.97,1.7,0.46));
#14003=CARTESIAN_POINT('',(1.97,1.7,0.46));
#14004=CARTESIAN_POINT('',(1.97,1.7,0.46));
#14005=CARTESIAN_POINT('',(3.07,1.7,0.46));
#14006=CARTESIAN_POINT('',(3.07,1.7,0.46));
#14007=CARTESIAN_POINT('',(1.97,1.7,0.46));
#14008=CARTESIAN_POINT('Origin',(1.97,0.78,0.46));
#14009=CARTESIAN_POINT('',(1.97,0.78,0.46));
#14010=CARTESIAN_POINT('',(1.97,0.78,0.46));
#14011=CARTESIAN_POINT('',(3.07,0.78,0.46));
#14012=CARTESIAN_POINT('',(3.07,0.78,0.46));
#14013=CARTESIAN_POINT('',(1.97,0.78,0.46));
#14014=CARTESIAN_POINT('Origin',(1.97,0.78,1.55));
#14015=CARTESIAN_POINT('',(1.97,0.78,1.55));
#14016=CARTESIAN_POINT('',(1.97,0.78,1.55));
#14017=CARTESIAN_POINT('',(3.07,0.78,1.55));
#14018=CARTESIAN_POINT('',(3.07,0.78,1.55));
#14019=CARTESIAN_POINT('',(1.97,0.78,1.55));
#14020=CARTESIAN_POINT('Origin',(1.97,-0.78,1.55));
#14021=CARTESIAN_POINT('',(1.97,-0.78,1.55));
#14022=CARTESIAN_POINT('',(1.97,-0.78,1.55));
#14023=CARTESIAN_POINT('',(3.07,-0.78,1.55));
#14024=CARTESIAN_POINT('',(3.07,-0.78,1.55));
#14025=CARTESIAN_POINT('',(1.97,-0.78,1.55));
#14026=CARTESIAN_POINT('Origin',(1.97,-0.78,0.46));
#14027=CARTESIAN_POINT('',(1.97,-0.78,0.46));
#14028=CARTESIAN_POINT('',(1.97,-0.78,0.46));
#14029=CARTESIAN_POINT('',(3.07,-0.78,0.46));
#14030=CARTESIAN_POINT('',(3.07,-0.78,0.46));
#14031=CARTESIAN_POINT('',(1.97,-0.78,0.46));
#14032=CARTESIAN_POINT('Origin',(1.97,-1.7,0.46));
#14033=CARTESIAN_POINT('',(1.97,-1.7,0.46));
#14034=CARTESIAN_POINT('',(1.97,-1.7,0.46));
#14035=CARTESIAN_POINT('',(3.07,-1.7,0.46));
#14036=CARTESIAN_POINT('',(3.07,-1.7,0.46));
#14037=CARTESIAN_POINT('',(1.97,-1.7,0.46));
#14038=CARTESIAN_POINT('Origin',(1.97,-1.7,2.3));
#14039=CARTESIAN_POINT('',(1.97,-1.7,2.3));
#14040=CARTESIAN_POINT('',(3.07,-1.7,2.3));
#14041=CARTESIAN_POINT('Origin',(3.07,0.,1.38));
#14042=CARTESIAN_POINT('Origin',(1.97,0.,1.38));
#14043=CARTESIAN_POINT('',(0.,0.,0.));
#14044=CARTESIAN_POINT('Origin',(-1.97,-0.78,0.46));
#14045=CARTESIAN_POINT('',(-1.97,-1.7,0.46));
#14046=CARTESIAN_POINT('',(-1.97,-0.78,0.46));
#14047=CARTESIAN_POINT('',(-1.97,-1.7,0.46));
#14048=CARTESIAN_POINT('',(-3.07,-1.7,0.46));
#14049=CARTESIAN_POINT('',(-1.97,-1.7,0.46));
#14050=CARTESIAN_POINT('',(-3.07,-0.78,0.46));
#14051=CARTESIAN_POINT('',(-3.07,-1.7,0.46));
#14052=CARTESIAN_POINT('',(-1.97,-0.78,0.46));
#14053=CARTESIAN_POINT('Origin',(-1.97,-0.78,1.55));
#14054=CARTESIAN_POINT('',(-1.97,-0.78,1.55));
#14055=CARTESIAN_POINT('',(-1.97,-0.78,0.46));
#14056=CARTESIAN_POINT('',(-3.07,-0.78,1.55));
#14057=CARTESIAN_POINT('',(-3.07,-0.78,0.46));
#14058=CARTESIAN_POINT('',(-1.97,-0.78,1.55));
#14059=CARTESIAN_POINT('Origin',(-1.97,0.78,1.55));
#14060=CARTESIAN_POINT('',(-1.97,0.78,1.55));
#14061=CARTESIAN_POINT('',(-1.97,-0.78,1.55));
#14062=CARTESIAN_POINT('',(-3.07,0.78,1.55));
#14063=CARTESIAN_POINT('',(-3.07,-0.78,1.55));
#14064=CARTESIAN_POINT('',(-1.97,0.78,1.55));
#14065=CARTESIAN_POINT('Origin',(-1.97,0.78,0.46));
#14066=CARTESIAN_POINT('',(-1.97,0.78,0.46));
#14067=CARTESIAN_POINT('',(-1.97,0.78,1.55));
#14068=CARTESIAN_POINT('',(-3.07,0.78,0.46));
#14069=CARTESIAN_POINT('',(-3.07,0.78,1.55));
#14070=CARTESIAN_POINT('',(-1.97,0.78,0.46));
#14071=CARTESIAN_POINT('Origin',(-1.97,1.7,0.46));
#14072=CARTESIAN_POINT('',(-1.97,1.7,0.46));
#14073=CARTESIAN_POINT('',(-1.97,0.78,0.46));
#14074=CARTESIAN_POINT('',(-3.07,1.7,0.46));
#14075=CARTESIAN_POINT('',(-3.07,0.78,0.46));
#14076=CARTESIAN_POINT('',(-1.97,1.7,0.46));
#14077=CARTESIAN_POINT('Origin',(-1.97,1.7,2.3));
#14078=CARTESIAN_POINT('',(-1.97,1.7,2.3));
#14079=CARTESIAN_POINT('',(-1.97,1.7,0.46));
#14080=CARTESIAN_POINT('',(-3.07,1.7,2.3));
#14081=CARTESIAN_POINT('',(-3.07,1.7,0.46));
#14082=CARTESIAN_POINT('',(-1.97,1.7,2.3));
#14083=CARTESIAN_POINT('Origin',(-1.97,-1.7,2.3));
#14084=CARTESIAN_POINT('',(-1.97,-1.7,2.3));
#14085=CARTESIAN_POINT('',(-1.97,1.7,2.3));
#14086=CARTESIAN_POINT('',(-3.07,-1.7,2.3));
#14087=CARTESIAN_POINT('',(-3.07,1.7,2.3));
#14088=CARTESIAN_POINT('',(-1.97,-1.7,2.3));
#14089=CARTESIAN_POINT('Origin',(-1.97,-1.7,0.46));
#14090=CARTESIAN_POINT('',(-1.97,-1.7,2.3));
#14091=CARTESIAN_POINT('',(-3.07,-1.7,2.3));
#14092=CARTESIAN_POINT('Origin',(-1.97,0.,1.38));
#14093=CARTESIAN_POINT('Origin',(-3.07,0.,1.38));
#14094=CARTESIAN_POINT('',(0.,0.,0.));
#14095=CARTESIAN_POINT('',(0.,0.,0.));
#14096=CARTESIAN_POINT('',(0.,0.,0.));
#14097=CARTESIAN_POINT('',(0.,0.,0.));
#14098=CARTESIAN_POINT('Origin',(0.,0.09,0.));
#14099=CARTESIAN_POINT('',(-0.285,0.1,3.49024337756996E-17));
#14100=CARTESIAN_POINT('Origin',(0.,0.1,0.));
#14101=CARTESIAN_POINT('',(-0.265,0.08,-3.24531401774049E-17));
#14102=CARTESIAN_POINT('',(-0.275,0.09,3.36777869765522E-17));
#14103=CARTESIAN_POINT('Origin',(0.,0.08,0.));
#14104=CARTESIAN_POINT('Origin',(0.,0.,0.));
#14105=CARTESIAN_POINT('',(-0.265,0.,3.24531401774049E-17));
#14106=CARTESIAN_POINT('',(-0.265,0.,3.24531401774049E-17));
#14107=CARTESIAN_POINT('Origin',(0.,0.,0.));
#14108=CARTESIAN_POINT('Origin',(0.,0.1,0.));
#14109=CARTESIAN_POINT('',(-0.5,0.1,6.12323399573677E-17));
#14110=CARTESIAN_POINT('Origin',(0.,0.1,0.));
#14111=CARTESIAN_POINT('Origin',(0.,0.,0.));
#14112=CARTESIAN_POINT('',(-0.5,0.,6.12323399573677E-17));
#14113=CARTESIAN_POINT('',(-0.5,0.,6.12323399573677E-17));
#14114=CARTESIAN_POINT('Origin',(0.,0.,0.));
#14115=CARTESIAN_POINT('Origin',(0.,0.,0.));
#14116=CARTESIAN_POINT('',(0.,0.,0.));
#14117=CARTESIAN_POINT('Origin',(0.375,0.5,0.));
#14118=CARTESIAN_POINT('',(-0.375,0.5,-4.59242549680257E-17));
#14119=CARTESIAN_POINT('Origin',(0.,0.5,0.));
#14120=CARTESIAN_POINT('Origin',(0.,0.475,0.));
#14121=CARTESIAN_POINT('',(-0.425,0.45,-5.20474889637625E-17));
#14122=CARTESIAN_POINT('Origin',(0.,0.45,0.));
#14123=CARTESIAN_POINT('',(-0.4,0.475,-4.89858719658941E-17));
#14124=CARTESIAN_POINT('Origin',(0.,0.24,0.));
#14125=CARTESIAN_POINT('',(-0.425,0.0299999999999998,-5.20474889637625E-17));
#14126=CARTESIAN_POINT('Origin',(0.,0.0299999999999998,0.));
#14127=CARTESIAN_POINT('',(-0.425,0.24,-5.20474889637625E-17));
#14128=CARTESIAN_POINT('Origin',(0.,0.0150000000000001,0.));
#14129=CARTESIAN_POINT('',(-0.395,4.85722573273506E-17,-4.83735485663204E-17));
#14130=CARTESIAN_POINT('Origin',(0.,0.,0.));
#14131=CARTESIAN_POINT('',(-0.41,0.0150000000000001,-5.02105187650415E-17));
#14132=CARTESIAN_POINT('Origin',(0.27,0.,0.));
#14133=CARTESIAN_POINT('',(-0.27,0.,-3.30654635769785E-17));
#14134=CARTESIAN_POINT('Origin',(0.,0.,0.));
#14135=CARTESIAN_POINT('Origin',(0.,-0.02,0.));
#14136=CARTESIAN_POINT('',(-0.24505,-0.0498999999999999,3.00099698131059E-17));
#14137=CARTESIAN_POINT('Origin',(0.,-0.0498999999999999,0.));
#14138=CARTESIAN_POINT('',(-0.26,-0.02,-3.18408167778312E-17));
#14139=CARTESIAN_POINT('Origin',(0.,-0.995,0.));
#14140=CARTESIAN_POINT('',(-0.24505,-1.95495,3.00099698131059E-17));
#14141=CARTESIAN_POINT('Origin',(0.,-1.95495,0.));
#14142=CARTESIAN_POINT('',(-0.24505,-0.995,-3.00099698131059E-17));
#14143=CARTESIAN_POINT('Origin',(0.,-1.975,0.));
#14144=CARTESIAN_POINT('',(-0.2,-2.,-2.44929359829471E-17));
#14145=CARTESIAN_POINT('Origin',(0.,-2.,0.));
#14146=CARTESIAN_POINT('',(-0.225,-1.975,-2.75545529808154E-17));
#14147=CARTESIAN_POINT('Origin',(0.,-2.,0.));
#14148=CARTESIAN_POINT('Origin',(0.115470053837925,-0.5,-0.2));
#14149=CARTESIAN_POINT('',(0.23094010767585,-0.5,0.));
#14150=CARTESIAN_POINT('',(0.115470053837925,-0.5,-0.2));
#14151=CARTESIAN_POINT('',(0.23094010767585,-0.5,0.));
#14152=CARTESIAN_POINT('',(0.115470053837925,-0.8,-0.2));
#14153=CARTESIAN_POINT('',(0.115470053837925,-0.5,-0.2));
#14154=CARTESIAN_POINT('',(0.23094010767585,-0.8,0.));
#14155=CARTESIAN_POINT('',(0.23094010767585,-0.8,0.));
#14156=CARTESIAN_POINT('',(0.23094010767585,-0.5,0.));
#14157=CARTESIAN_POINT('Origin',(-0.115470053837925,-0.5,-0.2));
#14158=CARTESIAN_POINT('',(-0.115470053837925,-0.5,-0.2));
#14159=CARTESIAN_POINT('',(0.115470053837925,-0.5,-0.2));
#14160=CARTESIAN_POINT('',(-0.115470053837925,-0.8,-0.2));
#14161=CARTESIAN_POINT('',(-0.115470053837925,-0.5,-0.2));
#14162=CARTESIAN_POINT('',(0.115470053837925,-0.8,-0.2));
#14163=CARTESIAN_POINT('Origin',(-0.23094010767585,-0.5,-2.77555756156289E-17));
#14164=CARTESIAN_POINT('',(-0.23094010767585,-0.5,-2.82820063659975E-17));
#14165=CARTESIAN_POINT('',(-0.115470053837925,-0.5,-0.2));
#14166=CARTESIAN_POINT('',(-0.23094010767585,-0.8,-2.77555756156289E-17));
#14167=CARTESIAN_POINT('',(-0.23094010767585,-0.5,-2.82820063659975E-17));
#14168=CARTESIAN_POINT('',(-0.115470053837925,-0.8,-0.2));
#14169=CARTESIAN_POINT('Origin',(-0.115470053837925,-0.5,0.2));
#14170=CARTESIAN_POINT('',(-0.115470053837925,-0.5,0.2));
#14171=CARTESIAN_POINT('',(-0.23094010767585,-0.5,-2.82820063659975E-17));
#14172=CARTESIAN_POINT('',(-0.115470053837925,-0.8,0.2));
#14173=CARTESIAN_POINT('',(-0.115470053837925,-0.5,0.2));
#14174=CARTESIAN_POINT('',(-0.23094010767585,-0.8,-2.82820063659975E-17));
#14175=CARTESIAN_POINT('Origin',(0.115470053837925,-0.5,0.2));
#14176=CARTESIAN_POINT('',(0.115470053837925,-0.5,0.2));
#14177=CARTESIAN_POINT('',(-0.115470053837925,-0.5,0.2));
#14178=CARTESIAN_POINT('',(0.115470053837925,-0.8,0.2));
#14179=CARTESIAN_POINT('',(0.115470053837925,-0.5,0.2));
#14180=CARTESIAN_POINT('',(-0.115470053837925,-0.8,0.2));
#14181=CARTESIAN_POINT('Origin',(0.23094010767585,-0.5,0.));
#14182=CARTESIAN_POINT('',(0.115470053837925,-0.5,0.2));
#14183=CARTESIAN_POINT('',(0.115470053837925,-0.8,0.2));
#14184=CARTESIAN_POINT('Origin',(0.,-0.5,0.));
#14185=CARTESIAN_POINT('Origin',(0.,-0.8,0.));
#14186=CARTESIAN_POINT('',(0.,0.,0.));
#14187=CARTESIAN_POINT('Origin',(0.,0.07,0.));
#14188=CARTESIAN_POINT('',(-0.235,0.08,2.87791997799628E-17));
#14189=CARTESIAN_POINT('Origin',(0.,0.08,0.));
#14190=CARTESIAN_POINT('',(-0.215,0.06,-2.63299061816681E-17));
#14191=CARTESIAN_POINT('',(-0.225,0.07,2.75545529808154E-17));
#14192=CARTESIAN_POINT('Origin',(0.,0.06,0.));
#14193=CARTESIAN_POINT('Origin',(0.,0.,0.));
#14194=CARTESIAN_POINT('',(-0.215,0.,2.63299061816681E-17));
#14195=CARTESIAN_POINT('',(-0.215,0.,2.63299061816681E-17));
#14196=CARTESIAN_POINT('Origin',(0.,0.,0.));
#14197=CARTESIAN_POINT('Origin',(0.,0.08,0.));
#14198=CARTESIAN_POINT('',(-0.45,0.08,5.51091059616309E-17));
#14199=CARTESIAN_POINT('Origin',(0.,0.08,0.));
#14200=CARTESIAN_POINT('Origin',(0.,0.,0.));
#14201=CARTESIAN_POINT('',(-0.45,0.,5.51091059616309E-17));
#14202=CARTESIAN_POINT('',(-0.45,0.,5.51091059616309E-17));
#14203=CARTESIAN_POINT('Origin',(0.,0.,0.));
#14204=CARTESIAN_POINT('Origin',(0.,0.,0.));
#14205=CARTESIAN_POINT('',(0.,0.,0.));
#14206=CARTESIAN_POINT('Origin',(0.3,0.4,0.));
#14207=CARTESIAN_POINT('',(-0.3,0.4,-3.67394039744206E-17));
#14208=CARTESIAN_POINT('Origin',(0.,0.4,0.));
#14209=CARTESIAN_POINT('Origin',(0.,0.375,0.));
#14210=CARTESIAN_POINT('',(-0.35,0.35,-4.28626379701573E-17));
#14211=CARTESIAN_POINT('Origin',(0.,0.35,0.));
#14212=CARTESIAN_POINT('',(-0.325,0.375,-3.9801020972289E-17));
#14213=CARTESIAN_POINT('Origin',(0.,0.19,0.));
#14214=CARTESIAN_POINT('',(-0.35,0.03,-4.28626379701574E-17));
#14215=CARTESIAN_POINT('Origin',(0.,0.03,0.));
#14216=CARTESIAN_POINT('',(-0.35,0.19,-4.28626379701574E-17));
#14217=CARTESIAN_POINT('Origin',(0.,0.0149999999999999,0.));
#14218=CARTESIAN_POINT('',(-0.32,-3.29597460435593E-17,-3.91886975727153E-17));
#14219=CARTESIAN_POINT('Origin',(0.,0.,0.));
#14220=CARTESIAN_POINT('',(-0.335,0.0149999999999999,-4.10256677714363E-17));
#14221=CARTESIAN_POINT('Origin',(0.22,0.,0.));
#14222=CARTESIAN_POINT('',(-0.22,-6.93889390390723E-18,-2.69422295812418E-17));
#14223=CARTESIAN_POINT('Origin',(0.,0.,0.));
#14224=CARTESIAN_POINT('Origin',(0.,-0.02,0.));
#14225=CARTESIAN_POINT('',(-0.1954,-0.0492,2.39295984553393E-17));
#14226=CARTESIAN_POINT('Origin',(0.,-0.0492,0.));
#14227=CARTESIAN_POINT('',(-0.21,-0.02,-2.57175827820944E-17));
#14228=CARTESIAN_POINT('Origin',(0.,-0.8,0.));
#14229=CARTESIAN_POINT('',(-0.1954,-1.5646,2.39295984553393E-17));
#14230=CARTESIAN_POINT('Origin',(0.,-1.5646,0.));
#14231=CARTESIAN_POINT('',(-0.1954,-0.8,-2.39295984553393E-17));
#14232=CARTESIAN_POINT('Origin',(0.,-1.58,0.));
#14233=CARTESIAN_POINT('',(-0.16,-1.6,-1.95943487863577E-17));
#14234=CARTESIAN_POINT('Origin',(0.,-1.6,0.));
#14235=CARTESIAN_POINT('',(-0.18,-1.58,-2.20436423846524E-17));
#14236=CARTESIAN_POINT('Origin',(0.,-1.6,0.));
#14237=CARTESIAN_POINT('Origin',(0.0866025403784439,-0.4,-0.15));
#14238=CARTESIAN_POINT('',(0.173205080756888,-0.4,0.));
#14239=CARTESIAN_POINT('',(0.0866025403784439,-0.4,-0.15));
#14240=CARTESIAN_POINT('',(0.173205080756888,-0.4,0.));
#14241=CARTESIAN_POINT('',(0.0866025403784439,-0.64,-0.15));
#14242=CARTESIAN_POINT('',(0.0866025403784439,-0.4,-0.15));
#14243=CARTESIAN_POINT('',(0.173205080756888,-0.64,0.));
#14244=CARTESIAN_POINT('',(0.173205080756888,-0.64,0.));
#14245=CARTESIAN_POINT('',(0.173205080756888,-0.4,0.));
#14246=CARTESIAN_POINT('Origin',(-0.0866025403784438,-0.4,-0.15));
#14247=CARTESIAN_POINT('',(-0.0866025403784438,-0.4,-0.15));
#14248=CARTESIAN_POINT('',(0.0866025403784439,-0.4,-0.15));
#14249=CARTESIAN_POINT('',(-0.0866025403784438,-0.64,-0.15));
#14250=CARTESIAN_POINT('',(-0.0866025403784438,-0.4,-0.15));
#14251=CARTESIAN_POINT('',(0.0866025403784439,-0.64,-0.15));
#14252=CARTESIAN_POINT('Origin',(-0.173205080756888,-0.4,-2.77555756156289E-17));
#14253=CARTESIAN_POINT('',(-0.173205080756888,-0.4,-2.12115047744981E-17));
#14254=CARTESIAN_POINT('',(-0.0866025403784438,-0.4,-0.15));
#14255=CARTESIAN_POINT('',(-0.173205080756888,-0.64,-2.77555756156289E-17));
#14256=CARTESIAN_POINT('',(-0.173205080756888,-0.4,-2.12115047744981E-17));
#14257=CARTESIAN_POINT('',(-0.0866025403784438,-0.64,-0.15));
#14258=CARTESIAN_POINT('Origin',(-0.0866025403784439,-0.4,0.15));
#14259=CARTESIAN_POINT('',(-0.0866025403784439,-0.4,0.15));
#14260=CARTESIAN_POINT('',(-0.173205080756888,-0.4,-2.12115047744981E-17));
#14261=CARTESIAN_POINT('',(-0.0866025403784439,-0.64,0.15));
#14262=CARTESIAN_POINT('',(-0.0866025403784439,-0.4,0.15));
#14263=CARTESIAN_POINT('',(-0.173205080756888,-0.64,-2.12115047744981E-17));
#14264=CARTESIAN_POINT('Origin',(0.0866025403784439,-0.4,0.15));
#14265=CARTESIAN_POINT('',(0.0866025403784439,-0.4,0.15));
#14266=CARTESIAN_POINT('',(-0.0866025403784439,-0.4,0.15));
#14267=CARTESIAN_POINT('',(0.0866025403784439,-0.64,0.15));
#14268=CARTESIAN_POINT('',(0.0866025403784439,-0.4,0.15));
#14269=CARTESIAN_POINT('',(-0.0866025403784439,-0.64,0.15));
#14270=CARTESIAN_POINT('Origin',(0.173205080756888,-0.4,0.));
#14271=CARTESIAN_POINT('',(0.0866025403784439,-0.4,0.15));
#14272=CARTESIAN_POINT('',(0.0866025403784439,-0.64,0.15));
#14273=CARTESIAN_POINT('Origin',(0.,-0.4,-2.77555756156289E-17));
#14274=CARTESIAN_POINT('Origin',(0.,-0.64,-2.77555756156289E-17));
#14275=CARTESIAN_POINT('',(0.,0.,0.));
#14276=CARTESIAN_POINT('',(0.,0.,0.));
#14277=CARTESIAN_POINT('',(0.,0.,0.));
#14278=CARTESIAN_POINT('',(0.,0.,0.));
#14279=CARTESIAN_POINT('',(0.,0.,0.));
#14280=CARTESIAN_POINT('',(0.,0.,0.));
#14281=CARTESIAN_POINT('',(0.,0.,0.));
#14282=CARTESIAN_POINT('',(0.,0.,0.));
#14283=CARTESIAN_POINT('',(0.,0.,0.));
#14284=CARTESIAN_POINT('',(0.,0.,0.));
#14285=CARTESIAN_POINT('',(0.,0.,2.8));
#14286=CARTESIAN_POINT('',(1.,-3.5,1.));
#14287=CARTESIAN_POINT('',(1.,3.5,1.));
#14288=CARTESIAN_POINT('',(2.5,-3.5,1.42));
#14289=CARTESIAN_POINT('',(2.5,-3.5,2.8));
#14290=CARTESIAN_POINT('',(2.5,-3.5,2.9));
#14291=CARTESIAN_POINT('',(2.5,3.5,1.42));
#14292=CARTESIAN_POINT('',(2.5,3.5,2.8));
#14293=CARTESIAN_POINT('',(2.5,3.5,2.9));
#14294=CARTESIAN_POINT('',(19.5,-3.5,1.42));
#14295=CARTESIAN_POINT('',(19.5,-3.5,2.8));
#14296=CARTESIAN_POINT('',(19.5,-3.5,2.9));
#14297=CARTESIAN_POINT('',(19.5,3.5,1.42));
#14298=CARTESIAN_POINT('',(19.5,3.5,2.8));
#14299=CARTESIAN_POINT('',(19.5,3.5,2.9));
#14300=CARTESIAN_POINT('',(2.,0.,3.77));
#14301=CARTESIAN_POINT('',(8.,0.,3.77));
#14302=CARTESIAN_POINT('',(14.,0.,3.77));
#14303=CARTESIAN_POINT('',(20.,0.,3.77));
#14304=CARTESIAN_POINT('',(-1.,-2.4,4.));
#14305=CARTESIAN_POINT('',(-1.,2.4,4.));
#14306=CARTESIAN_POINT('',(23.,-2.4,4.));
#14307=CARTESIAN_POINT('',(23.,2.4,4.));
#14308=CARTESIAN_POINT('',(2.,4.4,3.));
#14309=CARTESIAN_POINT('',(2.,4.4,3.08));
#14310=CARTESIAN_POINT('',(20.,4.4,3.));
#14311=CARTESIAN_POINT('',(20.,4.4,3.08));
#14312=CARTESIAN_POINT('',(0.,0.,0.));
#14313=CARTESIAN_POINT('Origin',(0.,0.,0.));
#14314=CARTESIAN_POINT('',(-0.32,0.16,3.91886975727153E-17));
#14315=CARTESIAN_POINT('Origin',(0.,0.16,0.));
#14316=CARTESIAN_POINT('',(-0.32,0.,3.91886975727153E-17));
#14317=CARTESIAN_POINT('',(-0.32,0.,3.91886975727153E-17));
#14318=CARTESIAN_POINT('Origin',(0.,0.,0.));
#14319=CARTESIAN_POINT('Origin',(0.,0.,0.));
#14320=CARTESIAN_POINT('',(-0.6,0.16,7.34788079488412E-17));
#14321=CARTESIAN_POINT('Origin',(0.,0.16,0.));
#14322=CARTESIAN_POINT('',(-0.6,0.,7.34788079488412E-17));
#14323=CARTESIAN_POINT('',(-0.6,0.,7.34788079488412E-17));
#14324=CARTESIAN_POINT('Origin',(0.,0.,0.));
#14325=CARTESIAN_POINT('Origin',(0.,0.16,0.));
#14326=CARTESIAN_POINT('Origin',(0.,0.,0.));
#14327=CARTESIAN_POINT('',(0.,0.,0.));
#14328=CARTESIAN_POINT('Origin',(0.45,0.6,0.));
#14329=CARTESIAN_POINT('',(-0.45,0.6,-5.51091059616309E-17));
#14330=CARTESIAN_POINT('Origin',(0.,0.6,0.));
#14331=CARTESIAN_POINT('Origin',(0.,0.575,0.));
#14332=CARTESIAN_POINT('',(-0.5,0.55,-6.12323399573677E-17));
#14333=CARTESIAN_POINT('Origin',(0.,0.55,0.));
#14334=CARTESIAN_POINT('',(-0.475,0.575,-5.81707229594993E-17));
#14335=CARTESIAN_POINT('Origin',(0.,0.29,0.));
#14336=CARTESIAN_POINT('',(-0.5,0.0299999999999998,-6.12323399573677E-17));
#14337=CARTESIAN_POINT('Origin',(0.,0.0299999999999998,0.));
#14338=CARTESIAN_POINT('',(-0.5,0.29,-6.12323399573677E-17));
#14339=CARTESIAN_POINT('Origin',(0.,0.0150000000000001,0.));
#14340=CARTESIAN_POINT('',(-0.47,7.11236625150491E-17,-5.75583995599256E-17));
#14341=CARTESIAN_POINT('Origin',(0.,0.,0.));
#14342=CARTESIAN_POINT('',(-0.485,0.0150000000000001,-5.93953697586466E-17));
#14343=CARTESIAN_POINT('Origin',(0.32,0.,0.));
#14344=CARTESIAN_POINT('',(-0.32,-6.93889390390723E-18,-3.91886975727153E-17));
#14345=CARTESIAN_POINT('Origin',(0.,0.,0.));
#14346=CARTESIAN_POINT('Origin',(0.,-0.02,0.));
#14347=CARTESIAN_POINT('',(-0.2942,-0.0515999999999999,3.60291088309151E-17));
#14348=CARTESIAN_POINT('Origin',(0.,-0.0515999999999999,0.));
#14349=CARTESIAN_POINT('',(-0.31,-0.02,-3.7964050773568E-17));
#14350=CARTESIAN_POINT('Origin',(0.,-1.24,0.));
#14351=CARTESIAN_POINT('',(-0.2942,-2.4458,3.60291088309151E-17));
#14352=CARTESIAN_POINT('Origin',(0.,-2.4458,0.));
#14353=CARTESIAN_POINT('',(-0.2942,-1.24,-3.60291088309151E-17));
#14354=CARTESIAN_POINT('Origin',(0.,-2.47,0.));
#14355=CARTESIAN_POINT('',(-0.24,-2.5,-2.93915231795365E-17));
#14356=CARTESIAN_POINT('Origin',(0.,-2.5,0.));
#14357=CARTESIAN_POINT('',(-0.27,-2.47,-3.30654635769785E-17));
#14358=CARTESIAN_POINT('Origin',(0.,-2.5,0.));
#14359=CARTESIAN_POINT('Origin',(0.144337567297406,-0.6,-0.25));
#14360=CARTESIAN_POINT('',(0.288675134594813,-0.6,0.));
#14361=CARTESIAN_POINT('',(0.144337567297406,-0.6,-0.25));
#14362=CARTESIAN_POINT('',(0.288675134594813,-0.6,0.));
#14363=CARTESIAN_POINT('',(0.144337567297406,-0.96,-0.25));
#14364=CARTESIAN_POINT('',(0.144337567297406,-0.6,-0.25));
#14365=CARTESIAN_POINT('',(0.288675134594813,-0.96,0.));
#14366=CARTESIAN_POINT('',(0.288675134594813,-0.96,0.));
#14367=CARTESIAN_POINT('',(0.288675134594813,-0.6,0.));
#14368=CARTESIAN_POINT('Origin',(-0.144337567297406,-0.6,-0.25));
#14369=CARTESIAN_POINT('',(-0.144337567297406,-0.6,-0.25));
#14370=CARTESIAN_POINT('',(0.144337567297406,-0.6,-0.25));
#14371=CARTESIAN_POINT('',(-0.144337567297406,-0.96,-0.25));
#14372=CARTESIAN_POINT('',(-0.144337567297406,-0.6,-0.25));
#14373=CARTESIAN_POINT('',(0.144337567297406,-0.96,-0.25));
#14374=CARTESIAN_POINT('Origin',(-0.288675134594813,-0.6,-8.32667268468867E-17));
#14375=CARTESIAN_POINT('',(-0.288675134594813,-0.6,-3.53525079574969E-17));
#14376=CARTESIAN_POINT('',(-0.144337567297406,-0.6,-0.25));
#14377=CARTESIAN_POINT('',(-0.288675134594813,-0.96,-5.55111512312578E-17));
#14378=CARTESIAN_POINT('',(-0.288675134594813,-0.6,-3.53525079574969E-17));
#14379=CARTESIAN_POINT('',(-0.144337567297406,-0.96,-0.25));
#14380=CARTESIAN_POINT('Origin',(-0.144337567297407,-0.6,0.25));
#14381=CARTESIAN_POINT('',(-0.144337567297407,-0.6,0.25));
#14382=CARTESIAN_POINT('',(-0.288675134594813,-0.6,-3.53525079574969E-17));
#14383=CARTESIAN_POINT('',(-0.144337567297407,-0.96,0.25));
#14384=CARTESIAN_POINT('',(-0.144337567297407,-0.6,0.25));
#14385=CARTESIAN_POINT('',(-0.288675134594813,-0.96,-3.53525079574969E-17));
#14386=CARTESIAN_POINT('Origin',(0.144337567297406,-0.6,0.25));
#14387=CARTESIAN_POINT('',(0.144337567297406,-0.6,0.25));
#14388=CARTESIAN_POINT('',(-0.144337567297407,-0.6,0.25));
#14389=CARTESIAN_POINT('',(0.144337567297406,-0.96,0.25));
#14390=CARTESIAN_POINT('',(0.144337567297406,-0.6,0.25));
#14391=CARTESIAN_POINT('',(-0.144337567297407,-0.96,0.25));
#14392=CARTESIAN_POINT('Origin',(0.288675134594813,-0.6,0.));
#14393=CARTESIAN_POINT('',(0.144337567297406,-0.6,0.25));
#14394=CARTESIAN_POINT('',(0.144337567297406,-0.96,0.25));
#14395=CARTESIAN_POINT('Origin',(0.,-0.6,0.));
#14396=CARTESIAN_POINT('Origin',(0.,-0.96,0.));
#14397=CARTESIAN_POINT('',(0.,0.,0.));
#14398=CARTESIAN_POINT('',(0.,0.,0.));
#14399=CARTESIAN_POINT('',(0.,0.,0.));
#14400=CARTESIAN_POINT('',(11.,0.,2.8));
#14401=CARTESIAN_POINT('',(9.5,-1.9,6.4));
#14402=CARTESIAN_POINT('',(9.5,-1.9,6.5));
#14403=CARTESIAN_POINT('',(9.5,1.9,6.4));
#14404=CARTESIAN_POINT('',(9.5,1.9,6.5));
#14405=CARTESIAN_POINT('',(12.5,-1.9,6.4));
#14406=CARTESIAN_POINT('',(12.5,-1.9,6.5));
#14407=CARTESIAN_POINT('',(12.5,1.9,6.4));
#14408=CARTESIAN_POINT('',(12.5,1.9,6.5));
#14409=CARTESIAN_POINT('',(11.,3.5,6.6));
#14410=CARTESIAN_POINT('',(11.,3.5,6.68));
#14411=CARTESIAN_POINT('',(11.,0.,8.4));
#14412=CARTESIAN_POINT('',(11.,0.,8.56));
#14413=CARTESIAN_POINT('',(0.,0.,0.));
#14414=CARTESIAN_POINT('',(0.,0.,0.));
#14415=UNCERTAINTY_MEASURE_WITH_UNIT(LENGTH_MEASURE(0.001),#14479,
'DISTANCE_ACCURACY_VALUE',
'Maximum model space distance between geometric entities at asserted c
onnectivities');
#14416=UNCERTAINTY_MEASURE_WITH_UNIT(LENGTH_MEASURE(0.001),#14479,
'DISTANCE_ACCURACY_VALUE',
'Maximum model space distance between geometric entities at asserted c
onnectivities');
#14417=UNCERTAINTY_MEASURE_WITH_UNIT(LENGTH_MEASURE(0.001),#14479,
'DISTANCE_ACCURACY_VALUE',
'Maximum model space distance between geometric entities at asserted c
onnectivities');
#14418=UNCERTAINTY_MEASURE_WITH_UNIT(LENGTH_MEASURE(0.001),#14479,
'DISTANCE_ACCURACY_VALUE',
'Maximum model space distance between geometric entities at asserted c
onnectivities');
#14419=UNCERTAINTY_MEASURE_WITH_UNIT(LENGTH_MEASURE(0.001),#14479,
'DISTANCE_ACCURACY_VALUE',
'Maximum model space distance between geometric entities at asserted c
onnectivities');
#14420=UNCERTAINTY_MEASURE_WITH_UNIT(LENGTH_MEASURE(0.001),#14479,
'DISTANCE_ACCURACY_VALUE',
'Maximum model space distance between geometric entities at asserted c
onnectivities');
#14421=UNCERTAINTY_MEASURE_WITH_UNIT(LENGTH_MEASURE(0.001),#14479,
'DISTANCE_ACCURACY_VALUE',
'Maximum model space distance between geometric entities at asserted c
onnectivities');
#14422=UNCERTAINTY_MEASURE_WITH_UNIT(LENGTH_MEASURE(0.001),#14479,
'DISTANCE_ACCURACY_VALUE',
'Maximum model space distance between geometric entities at asserted c
onnectivities');
#14423=UNCERTAINTY_MEASURE_WITH_UNIT(LENGTH_MEASURE(0.001),#14479,
'DISTANCE_ACCURACY_VALUE',
'Maximum model space distance between geometric entities at asserted c
onnectivities');
#14424=UNCERTAINTY_MEASURE_WITH_UNIT(LENGTH_MEASURE(0.001),#14479,
'DISTANCE_ACCURACY_VALUE',
'Maximum model space distance between geometric entities at asserted c
onnectivities');
#14425=UNCERTAINTY_MEASURE_WITH_UNIT(LENGTH_MEASURE(0.001),#14479,
'DISTANCE_ACCURACY_VALUE',
'Maximum model space distance between geometric entities at asserted c
onnectivities');
#14426=UNCERTAINTY_MEASURE_WITH_UNIT(LENGTH_MEASURE(0.001),#14479,
'DISTANCE_ACCURACY_VALUE',
'Maximum model space distance between geometric entities at asserted c
onnectivities');
#14427=UNCERTAINTY_MEASURE_WITH_UNIT(LENGTH_MEASURE(0.001),#14479,
'DISTANCE_ACCURACY_VALUE',
'Maximum model space distance between geometric entities at asserted c
onnectivities');
#14428=UNCERTAINTY_MEASURE_WITH_UNIT(LENGTH_MEASURE(0.001),#14479,
'DISTANCE_ACCURACY_VALUE',
'Maximum model space distance between geometric entities at asserted c
onnectivities');
#14429=UNCERTAINTY_MEASURE_WITH_UNIT(LENGTH_MEASURE(0.001),#14479,
'DISTANCE_ACCURACY_VALUE',
'Maximum model space distance between geometric entities at asserted c
onnectivities');
#14430=UNCERTAINTY_MEASURE_WITH_UNIT(LENGTH_MEASURE(0.001),#14479,
'DISTANCE_ACCURACY_VALUE',
'Maximum model space distance between geometric entities at asserted c
onnectivities');
#14431=UNCERTAINTY_MEASURE_WITH_UNIT(LENGTH_MEASURE(0.001),#14479,
'DISTANCE_ACCURACY_VALUE',
'Maximum model space distance between geometric entities at asserted c
onnectivities');
#14432=UNCERTAINTY_MEASURE_WITH_UNIT(LENGTH_MEASURE(0.001),#14479,
'DISTANCE_ACCURACY_VALUE',
'Maximum model space distance between geometric entities at asserted c
onnectivities');
#14433=UNCERTAINTY_MEASURE_WITH_UNIT(LENGTH_MEASURE(0.001),#14479,
'DISTANCE_ACCURACY_VALUE',
'Maximum model space distance between geometric entities at asserted c
onnectivities');
#14434=UNCERTAINTY_MEASURE_WITH_UNIT(LENGTH_MEASURE(0.001),#14479,
'DISTANCE_ACCURACY_VALUE',
'Maximum model space distance between geometric entities at asserted c
onnectivities');
#14435=UNCERTAINTY_MEASURE_WITH_UNIT(LENGTH_MEASURE(0.001),#14479,
'DISTANCE_ACCURACY_VALUE',
'Maximum model space distance between geometric entities at asserted c
onnectivities');
#14436=UNCERTAINTY_MEASURE_WITH_UNIT(LENGTH_MEASURE(0.001),#14479,
'DISTANCE_ACCURACY_VALUE',
'Maximum model space distance between geometric entities at asserted c
onnectivities');
#14437=UNCERTAINTY_MEASURE_WITH_UNIT(LENGTH_MEASURE(0.001),#14479,
'DISTANCE_ACCURACY_VALUE',
'Maximum model space distance between geometric entities at asserted c
onnectivities');
#14438=UNCERTAINTY_MEASURE_WITH_UNIT(LENGTH_MEASURE(0.001),#14479,
'DISTANCE_ACCURACY_VALUE',
'Maximum model space distance between geometric entities at asserted c
onnectivities');
#14439=UNCERTAINTY_MEASURE_WITH_UNIT(LENGTH_MEASURE(0.001),#14479,
'DISTANCE_ACCURACY_VALUE',
'Maximum model space distance between geometric entities at asserted c
onnectivities');
#14440=UNCERTAINTY_MEASURE_WITH_UNIT(LENGTH_MEASURE(0.001),#14479,
'DISTANCE_ACCURACY_VALUE',
'Maximum model space distance between geometric entities at asserted c
onnectivities');
#14441=UNCERTAINTY_MEASURE_WITH_UNIT(LENGTH_MEASURE(0.001),#14479,
'DISTANCE_ACCURACY_VALUE',
'Maximum model space distance between geometric entities at asserted c
onnectivities');
#14442=UNCERTAINTY_MEASURE_WITH_UNIT(LENGTH_MEASURE(0.001),#14479,
'DISTANCE_ACCURACY_VALUE',
'Maximum model space distance between geometric entities at asserted c
onnectivities');
#14443=UNCERTAINTY_MEASURE_WITH_UNIT(LENGTH_MEASURE(0.001),#14479,
'DISTANCE_ACCURACY_VALUE',
'Maximum model space distance between geometric entities at asserted c
onnectivities');
#14444=UNCERTAINTY_MEASURE_WITH_UNIT(LENGTH_MEASURE(0.001),#14479,
'DISTANCE_ACCURACY_VALUE',
'Maximum model space distance between geometric entities at asserted c
onnectivities');
#14445=UNCERTAINTY_MEASURE_WITH_UNIT(LENGTH_MEASURE(0.001),#14479,
'DISTANCE_ACCURACY_VALUE',
'Maximum model space distance between geometric entities at asserted c
onnectivities');
#14446=UNCERTAINTY_MEASURE_WITH_UNIT(LENGTH_MEASURE(0.001),#14479,
'DISTANCE_ACCURACY_VALUE',
'Maximum model space distance between geometric entities at asserted c
onnectivities');
#14447=(
GEOMETRIC_REPRESENTATION_CONTEXT(3)
GLOBAL_UNCERTAINTY_ASSIGNED_CONTEXT((#14415))
GLOBAL_UNIT_ASSIGNED_CONTEXT((#14479,#14481,#14482))
REPRESENTATION_CONTEXT('','3D')
);
#14448=(
GEOMETRIC_REPRESENTATION_CONTEXT(3)
GLOBAL_UNCERTAINTY_ASSIGNED_CONTEXT((#14416))
GLOBAL_UNIT_ASSIGNED_CONTEXT((#14479,#14481,#14482))
REPRESENTATION_CONTEXT('','3D')
);
#14449=(
GEOMETRIC_REPRESENTATION_CONTEXT(3)
GLOBAL_UNCERTAINTY_ASSIGNED_CONTEXT((#14417))
GLOBAL_UNIT_ASSIGNED_CONTEXT((#14479,#14481,#14482))
REPRESENTATION_CONTEXT('','3D')
);
#14450=(
GEOMETRIC_REPRESENTATION_CONTEXT(3)
GLOBAL_UNCERTAINTY_ASSIGNED_CONTEXT((#14418))
GLOBAL_UNIT_ASSIGNED_CONTEXT((#14479,#14481,#14482))
REPRESENTATION_CONTEXT('','3D')
);
#14451=(
GEOMETRIC_REPRESENTATION_CONTEXT(3)
GLOBAL_UNCERTAINTY_ASSIGNED_CONTEXT((#14419))
GLOBAL_UNIT_ASSIGNED_CONTEXT((#14479,#14481,#14482))
REPRESENTATION_CONTEXT('','3D')
);
#14452=(
GEOMETRIC_REPRESENTATION_CONTEXT(3)
GLOBAL_UNCERTAINTY_ASSIGNED_CONTEXT((#14420))
GLOBAL_UNIT_ASSIGNED_CONTEXT((#14479,#14481,#14482))
REPRESENTATION_CONTEXT('','3D')
);
#14453=(
GEOMETRIC_REPRESENTATION_CONTEXT(3)
GLOBAL_UNCERTAINTY_ASSIGNED_CONTEXT((#14421))
GLOBAL_UNIT_ASSIGNED_CONTEXT((#14479,#14481,#14482))
REPRESENTATION_CONTEXT('','3D')
);
#14454=(
GEOMETRIC_REPRESENTATION_CONTEXT(3)
GLOBAL_UNCERTAINTY_ASSIGNED_CONTEXT((#14422))
GLOBAL_UNIT_ASSIGNED_CONTEXT((#14479,#14481,#14482))
REPRESENTATION_CONTEXT('','3D')
);
#14455=(
GEOMETRIC_REPRESENTATION_CONTEXT(3)
GLOBAL_UNCERTAINTY_ASSIGNED_CONTEXT((#14423))
GLOBAL_UNIT_ASSIGNED_CONTEXT((#14479,#14481,#14482))
REPRESENTATION_CONTEXT('','3D')
);
#14456=(
GEOMETRIC_REPRESENTATION_CONTEXT(3)
GLOBAL_UNCERTAINTY_ASSIGNED_CONTEXT((#14424))
GLOBAL_UNIT_ASSIGNED_CONTEXT((#14479,#14481,#14482))
REPRESENTATION_CONTEXT('','3D')
);
#14457=(
GEOMETRIC_REPRESENTATION_CONTEXT(3)
GLOBAL_UNCERTAINTY_ASSIGNED_CONTEXT((#14425))
GLOBAL_UNIT_ASSIGNED_CONTEXT((#14479,#14481,#14482))
REPRESENTATION_CONTEXT('','3D')
);
#14458=(
GEOMETRIC_REPRESENTATION_CONTEXT(3)
GLOBAL_UNCERTAINTY_ASSIGNED_CONTEXT((#14426))
GLOBAL_UNIT_ASSIGNED_CONTEXT((#14479,#14481,#14482))
REPRESENTATION_CONTEXT('','3D')
);
#14459=(
GEOMETRIC_REPRESENTATION_CONTEXT(3)
GLOBAL_UNCERTAINTY_ASSIGNED_CONTEXT((#14427))
GLOBAL_UNIT_ASSIGNED_CONTEXT((#14479,#14481,#14482))
REPRESENTATION_CONTEXT('','3D')
);
#14460=(
GEOMETRIC_REPRESENTATION_CONTEXT(3)
GLOBAL_UNCERTAINTY_ASSIGNED_CONTEXT((#14428))
GLOBAL_UNIT_ASSIGNED_CONTEXT((#14479,#14481,#14482))
REPRESENTATION_CONTEXT('','3D')
);
#14461=(
GEOMETRIC_REPRESENTATION_CONTEXT(3)
GLOBAL_UNCERTAINTY_ASSIGNED_CONTEXT((#14429))
GLOBAL_UNIT_ASSIGNED_CONTEXT((#14479,#14481,#14482))
REPRESENTATION_CONTEXT('','3D')
);
#14462=(
GEOMETRIC_REPRESENTATION_CONTEXT(3)
GLOBAL_UNCERTAINTY_ASSIGNED_CONTEXT((#14430))
GLOBAL_UNIT_ASSIGNED_CONTEXT((#14479,#14481,#14482))
REPRESENTATION_CONTEXT('','3D')
);
#14463=(
GEOMETRIC_REPRESENTATION_CONTEXT(3)
GLOBAL_UNCERTAINTY_ASSIGNED_CONTEXT((#14431))
GLOBAL_UNIT_ASSIGNED_CONTEXT((#14479,#14481,#14482))
REPRESENTATION_CONTEXT('','3D')
);
#14464=(
GEOMETRIC_REPRESENTATION_CONTEXT(3)
GLOBAL_UNCERTAINTY_ASSIGNED_CONTEXT((#14432))
GLOBAL_UNIT_ASSIGNED_CONTEXT((#14479,#14481,#14482))
REPRESENTATION_CONTEXT('','3D')
);
#14465=(
GEOMETRIC_REPRESENTATION_CONTEXT(3)
GLOBAL_UNCERTAINTY_ASSIGNED_CONTEXT((#14433))
GLOBAL_UNIT_ASSIGNED_CONTEXT((#14479,#14481,#14482))
REPRESENTATION_CONTEXT('','3D')
);
#14466=(
GEOMETRIC_REPRESENTATION_CONTEXT(3)
GLOBAL_UNCERTAINTY_ASSIGNED_CONTEXT((#14434))
GLOBAL_UNIT_ASSIGNED_CONTEXT((#14479,#14481,#14482))
REPRESENTATION_CONTEXT('','3D')
);
#14467=(
GEOMETRIC_REPRESENTATION_CONTEXT(3)
GLOBAL_UNCERTAINTY_ASSIGNED_CONTEXT((#14435))
GLOBAL_UNIT_ASSIGNED_CONTEXT((#14479,#14481,#14482))
REPRESENTATION_CONTEXT('','3D')
);
#14468=(
GEOMETRIC_REPRESENTATION_CONTEXT(3)
GLOBAL_UNCERTAINTY_ASSIGNED_CONTEXT((#14436))
GLOBAL_UNIT_ASSIGNED_CONTEXT((#14479,#14481,#14482))
REPRESENTATION_CONTEXT('','3D')
);
#14469=(
GEOMETRIC_REPRESENTATION_CONTEXT(3)
GLOBAL_UNCERTAINTY_ASSIGNED_CONTEXT((#14437))
GLOBAL_UNIT_ASSIGNED_CONTEXT((#14479,#14481,#14482))
REPRESENTATION_CONTEXT('','3D')
);
#14470=(
GEOMETRIC_REPRESENTATION_CONTEXT(3)
GLOBAL_UNCERTAINTY_ASSIGNED_CONTEXT((#14438))
GLOBAL_UNIT_ASSIGNED_CONTEXT((#14479,#14481,#14482))
REPRESENTATION_CONTEXT('','3D')
);
#14471=(
GEOMETRIC_REPRESENTATION_CONTEXT(3)
GLOBAL_UNCERTAINTY_ASSIGNED_CONTEXT((#14439))
GLOBAL_UNIT_ASSIGNED_CONTEXT((#14479,#14481,#14482))
REPRESENTATION_CONTEXT('','3D')
);
#14472=(
GEOMETRIC_REPRESENTATION_CONTEXT(3)
GLOBAL_UNCERTAINTY_ASSIGNED_CONTEXT((#14440))
GLOBAL_UNIT_ASSIGNED_CONTEXT((#14479,#14481,#14482))
REPRESENTATION_CONTEXT('','3D')
);
#14473=(
GEOMETRIC_REPRESENTATION_CONTEXT(3)
GLOBAL_UNCERTAINTY_ASSIGNED_CONTEXT((#14441))
GLOBAL_UNIT_ASSIGNED_CONTEXT((#14479,#14481,#14482))
REPRESENTATION_CONTEXT('','3D')
);
#14474=(
GEOMETRIC_REPRESENTATION_CONTEXT(3)
GLOBAL_UNCERTAINTY_ASSIGNED_CONTEXT((#14442))
GLOBAL_UNIT_ASSIGNED_CONTEXT((#14479,#14481,#14482))
REPRESENTATION_CONTEXT('','3D')
);
#14475=(
GEOMETRIC_REPRESENTATION_CONTEXT(3)
GLOBAL_UNCERTAINTY_ASSIGNED_CONTEXT((#14443))
GLOBAL_UNIT_ASSIGNED_CONTEXT((#14479,#14481,#14482))
REPRESENTATION_CONTEXT('','3D')
);
#14476=(
GEOMETRIC_REPRESENTATION_CONTEXT(3)
GLOBAL_UNCERTAINTY_ASSIGNED_CONTEXT((#14444))
GLOBAL_UNIT_ASSIGNED_CONTEXT((#14479,#14481,#14482))
REPRESENTATION_CONTEXT('','3D')
);
#14477=(
GEOMETRIC_REPRESENTATION_CONTEXT(3)
GLOBAL_UNCERTAINTY_ASSIGNED_CONTEXT((#14445))
GLOBAL_UNIT_ASSIGNED_CONTEXT((#14479,#14481,#14482))
REPRESENTATION_CONTEXT('','3D')
);
#14478=(
GEOMETRIC_REPRESENTATION_CONTEXT(3)
GLOBAL_UNCERTAINTY_ASSIGNED_CONTEXT((#14446))
GLOBAL_UNIT_ASSIGNED_CONTEXT((#14479,#14481,#14482))
REPRESENTATION_CONTEXT('','3D')
);
#14479=(
LENGTH_UNIT()
NAMED_UNIT(*)
SI_UNIT(.CENTI.,.METRE.)
);
#14480=(
LENGTH_UNIT()
NAMED_UNIT(*)
SI_UNIT($,.METRE.)
);
#14481=(
NAMED_UNIT(*)
PLANE_ANGLE_UNIT()
SI_UNIT($,.RADIAN.)
);
#14482=(
NAMED_UNIT(*)
SI_UNIT($,.STERADIAN.)
SOLID_ANGLE_UNIT()
);
#14483=SHAPE_DEFINITION_REPRESENTATION(#14514,#14603);
#14484=SHAPE_DEFINITION_REPRESENTATION(#14515,#14604);
#14485=SHAPE_DEFINITION_REPRESENTATION(#14516,#14605);
#14486=SHAPE_DEFINITION_REPRESENTATION(#14517,#14606);
#14487=SHAPE_DEFINITION_REPRESENTATION(#14518,#14607);
#14488=SHAPE_DEFINITION_REPRESENTATION(#14519,#14608);
#14489=SHAPE_DEFINITION_REPRESENTATION(#14520,#14609);
#14490=SHAPE_DEFINITION_REPRESENTATION(#14521,#14610);
#14491=SHAPE_DEFINITION_REPRESENTATION(#14522,#14611);
#14492=SHAPE_DEFINITION_REPRESENTATION(#14523,#14612);
#14493=SHAPE_DEFINITION_REPRESENTATION(#14524,#14613);
#14494=SHAPE_DEFINITION_REPRESENTATION(#14525,#14614);
#14495=SHAPE_DEFINITION_REPRESENTATION(#14526,#14615);
#14496=SHAPE_DEFINITION_REPRESENTATION(#14527,#14616);
#14497=SHAPE_DEFINITION_REPRESENTATION(#14528,#14617);
#14498=SHAPE_DEFINITION_REPRESENTATION(#14529,#14618);
#14499=SHAPE_DEFINITION_REPRESENTATION(#14530,#14619);
#14500=SHAPE_DEFINITION_REPRESENTATION(#14531,#14620);
#14501=SHAPE_DEFINITION_REPRESENTATION(#14532,#14621);
#14502=SHAPE_DEFINITION_REPRESENTATION(#14533,#14622);
#14503=SHAPE_DEFINITION_REPRESENTATION(#14534,#14623);
#14504=SHAPE_DEFINITION_REPRESENTATION(#14535,#14624);
#14505=SHAPE_DEFINITION_REPRESENTATION(#14536,#14625);
#14506=SHAPE_DEFINITION_REPRESENTATION(#14537,#14626);
#14507=SHAPE_DEFINITION_REPRESENTATION(#14538,#14627);
#14508=SHAPE_DEFINITION_REPRESENTATION(#14542,#14628);
#14509=SHAPE_DEFINITION_REPRESENTATION(#14543,#14629);
#14510=SHAPE_DEFINITION_REPRESENTATION(#14544,#14630);
#14511=SHAPE_DEFINITION_REPRESENTATION(#14545,#14631);
#14512=SHAPE_DEFINITION_REPRESENTATION(#14583,#14632);
#14513=SHAPE_DEFINITION_REPRESENTATION(#14584,#14633);
#14514=PRODUCT_DEFINITION_SHAPE('',$,#14635);
#14515=PRODUCT_DEFINITION_SHAPE('',$,#14636);
#14516=PRODUCT_DEFINITION_SHAPE('',$,#14637);
#14517=PRODUCT_DEFINITION_SHAPE('',$,#14638);
#14518=PRODUCT_DEFINITION_SHAPE('',$,#14639);
#14519=PRODUCT_DEFINITION_SHAPE('',$,#14640);
#14520=PRODUCT_DEFINITION_SHAPE('',$,#14641);
#14521=PRODUCT_DEFINITION_SHAPE('',$,#14642);
#14522=PRODUCT_DEFINITION_SHAPE('',$,#14643);
#14523=PRODUCT_DEFINITION_SHAPE('',$,#14644);
#14524=PRODUCT_DEFINITION_SHAPE('',$,#14645);
#14525=PRODUCT_DEFINITION_SHAPE('',$,#14646);
#14526=PRODUCT_DEFINITION_SHAPE('',$,#14647);
#14527=PRODUCT_DEFINITION_SHAPE('',$,#14648);
#14528=PRODUCT_DEFINITION_SHAPE('',$,#14649);
#14529=PRODUCT_DEFINITION_SHAPE('',$,#14650);
#14530=PRODUCT_DEFINITION_SHAPE('',$,#14651);
#14531=PRODUCT_DEFINITION_SHAPE('',$,#14652);
#14532=PRODUCT_DEFINITION_SHAPE('',$,#14653);
#14533=PRODUCT_DEFINITION_SHAPE('',$,#14654);
#14534=PRODUCT_DEFINITION_SHAPE('',$,#14655);
#14535=PRODUCT_DEFINITION_SHAPE('',$,#14656);
#14536=PRODUCT_DEFINITION_SHAPE('',$,#14657);
#14537=PRODUCT_DEFINITION_SHAPE('',$,#14658);
#14538=PRODUCT_DEFINITION_SHAPE('',$,#14659);
#14539=PRODUCT_DEFINITION_SHAPE($,$,#185);
#14540=PRODUCT_DEFINITION_SHAPE($,$,#186);
#14541=PRODUCT_DEFINITION_SHAPE($,$,#187);
#14542=PRODUCT_DEFINITION_SHAPE('',$,#14660);
#14543=PRODUCT_DEFINITION_SHAPE('',$,#14661);
#14544=PRODUCT_DEFINITION_SHAPE('',$,#14662);
#14545=PRODUCT_DEFINITION_SHAPE('',$,#14663);
#14546=PRODUCT_DEFINITION_SHAPE($,$,#188);
#14547=PRODUCT_DEFINITION_SHAPE($,$,#189);
#14548=PRODUCT_DEFINITION_SHAPE($,$,#190);
#14549=PRODUCT_DEFINITION_SHAPE($,$,#191);
#14550=PRODUCT_DEFINITION_SHAPE($,$,#192);
#14551=PRODUCT_DEFINITION_SHAPE($,$,#193);
#14552=PRODUCT_DEFINITION_SHAPE($,$,#194);
#14553=PRODUCT_DEFINITION_SHAPE($,$,#195);
#14554=PRODUCT_DEFINITION_SHAPE($,$,#196);
#14555=PRODUCT_DEFINITION_SHAPE($,$,#197);
#14556=PRODUCT_DEFINITION_SHAPE($,$,#198);
#14557=PRODUCT_DEFINITION_SHAPE($,$,#199);
#14558=PRODUCT_DEFINITION_SHAPE($,$,#200);
#14559=PRODUCT_DEFINITION_SHAPE($,$,#201);
#14560=PRODUCT_DEFINITION_SHAPE($,$,#202);
#14561=PRODUCT_DEFINITION_SHAPE($,$,#203);
#14562=PRODUCT_DEFINITION_SHAPE($,$,#204);
#14563=PRODUCT_DEFINITION_SHAPE($,$,#205);
#14564=PRODUCT_DEFINITION_SHAPE($,$,#206);
#14565=PRODUCT_DEFINITION_SHAPE($,$,#207);
#14566=PRODUCT_DEFINITION_SHAPE($,$,#208);
#14567=PRODUCT_DEFINITION_SHAPE($,$,#209);
#14568=PRODUCT_DEFINITION_SHAPE($,$,#210);
#14569=PRODUCT_DEFINITION_SHAPE($,$,#211);
#14570=PRODUCT_DEFINITION_SHAPE($,$,#212);
#14571=PRODUCT_DEFINITION_SHAPE($,$,#213);
#14572=PRODUCT_DEFINITION_SHAPE($,$,#214);
#14573=PRODUCT_DEFINITION_SHAPE($,$,#215);
#14574=PRODUCT_DEFINITION_SHAPE($,$,#216);
#14575=PRODUCT_DEFINITION_SHAPE($,$,#217);
#14576=PRODUCT_DEFINITION_SHAPE($,$,#218);
#14577=PRODUCT_DEFINITION_SHAPE($,$,#219);
#14578=PRODUCT_DEFINITION_SHAPE($,$,#220);
#14579=PRODUCT_DEFINITION_SHAPE($,$,#221);
#14580=PRODUCT_DEFINITION_SHAPE($,$,#222);
#14581=PRODUCT_DEFINITION_SHAPE($,$,#223);
#14582=PRODUCT_DEFINITION_SHAPE($,$,#224);
#14583=PRODUCT_DEFINITION_SHAPE('',$,#14664);
#14584=PRODUCT_DEFINITION_SHAPE('',$,#14665);
#14585=PRODUCT_DEFINITION_SHAPE($,$,#225);
#14586=PRODUCT_DEFINITION_SHAPE($,$,#226);
#14587=PRODUCT_DEFINITION_SHAPE($,$,#227);
#14588=PRODUCT_DEFINITION_SHAPE($,$,#228);
#14589=PRODUCT_DEFINITION_SHAPE($,$,#229);
#14590=PRODUCT_DEFINITION_SHAPE($,$,#230);
#14591=PRODUCT_DEFINITION_SHAPE($,$,#231);
#14592=PRODUCT_DEFINITION_SHAPE($,$,#232);
#14593=PRODUCT_DEFINITION_SHAPE($,$,#233);
#14594=PRODUCT_DEFINITION_SHAPE($,$,#234);
#14595=PRODUCT_DEFINITION_SHAPE($,$,#235);
#14596=PRODUCT_DEFINITION_SHAPE($,$,#236);
#14597=PRODUCT_DEFINITION_SHAPE($,$,#237);
#14598=PRODUCT_DEFINITION_SHAPE($,$,#238);
#14599=PRODUCT_DEFINITION_SHAPE($,$,#239);
#14600=PRODUCT_DEFINITION_SHAPE($,$,#240);
#14601=PRODUCT_DEFINITION_SHAPE($,$,#241);
#14602=PRODUCT_DEFINITION_SHAPE($,$,#242);
#14603=SHAPE_REPRESENTATION('',(#8919,#9619,#9620),#14447);
#14604=SHAPE_REPRESENTATION('',(#8920,#9531,#9532,#9533,#9534,#9535,#9536,
#9537,#9538,#9539,#9540,#9541,#9542,#9543,#9544,#9545,#9546,#9547,#9548,
#9549,#9550,#9551,#9552,#9553,#9554,#9555,#9556,#9557,#9558,#9559,#9560,
#9561,#9562,#9563,#9564,#9565,#9566,#9567),#14448);
#14605=SHAPE_REPRESENTATION('',(#8921),#14449);
#14606=SHAPE_REPRESENTATION('',(#8970),#14450);
#14607=SHAPE_REPRESENTATION('',(#8991),#14451);
#14608=SHAPE_REPRESENTATION('',(#8998),#14452);
#14609=SHAPE_REPRESENTATION('',(#9019),#14453);
#14610=SHAPE_REPRESENTATION('',(#9026),#14454);
#14611=SHAPE_REPRESENTATION('',(#9155),#14455);
#14612=SHAPE_REPRESENTATION('',(#9162),#14456);
#14613=SHAPE_REPRESENTATION('',(#9169),#14457);
#14614=SHAPE_REPRESENTATION('',(#9176),#14458);
#14615=SHAPE_REPRESENTATION('',(#9183),#14459);
#14616=SHAPE_REPRESENTATION('',(#9226),#14460);
#14617=SHAPE_REPRESENTATION('',(#9276),#14461);
#14618=SHAPE_REPRESENTATION('',(#9297),#14462);
#14619=SHAPE_REPRESENTATION('',(#9321),#14463);
#14620=SHAPE_REPRESENTATION('',(#9345,#9603,#9604,#9605,#9606,#9607,#9608,
#9609,#9610,#9611,#9612,#9613,#9614,#9615,#9616,#9617,#9618),#14464);
#14621=SHAPE_REPRESENTATION('',(#9346),#14465);
#14622=SHAPE_REPRESENTATION('',(#9371),#14466);
#14623=SHAPE_REPRESENTATION('',(#9383),#14467);
#14624=SHAPE_REPRESENTATION('',(#9392,#9454,#9455,#9456),#14468);
#14625=SHAPE_REPRESENTATION('',(#9393),#14469);
#14626=SHAPE_REPRESENTATION('',(#9432),#14470);
#14627=SHAPE_REPRESENTATION('',(#9443),#14471);
#14628=SHAPE_REPRESENTATION('',(#9457),#14472);
#14629=SHAPE_REPRESENTATION('',(#9468),#14473);
#14630=SHAPE_REPRESENTATION('',(#9494),#14474);
#14631=SHAPE_REPRESENTATION('',(#9505),#14475);
#14632=SHAPE_REPRESENTATION('',(#9568),#14476);
#14633=SHAPE_REPRESENTATION('',(#9577),#14477);
#14634=PRODUCT_DEFINITION_CONTEXT('part definition',#14729,'design');
#14635=PRODUCT_DEFINITION('PAT-095',
'PAT-095',#14666,#14634);
#14636=PRODUCT_DEFINITION('Stationary frame','Stationary frame',#14667,
#14634);
#14637=PRODUCT_DEFINITION('Base plate','Base plate',#14668,#14634);
#14638=PRODUCT_DEFINITION('End stop','End stop',#14669,#14634);
#14639=PRODUCT_DEFINITION('Bonded stop pad','Bonded stop pad',#14670,#14634);
#14640=PRODUCT_DEFINITION('End stop (1)','End stop (1)',#14671,#14634);
#14641=PRODUCT_DEFINITION('Bonded stop pad (1)','Bonded stop pad (1)',#14672,
#14634);
#14642=PRODUCT_DEFINITION('Graduated scale','Graduated scale',#14673,#14634);
#14643=PRODUCT_DEFINITION('Bonded foot pad','Bonded foot pad',#14674,#14634);
#14644=PRODUCT_DEFINITION('Bonded foot pad (1)','Bonded foot pad (1)',#14675,
#14634);
#14645=PRODUCT_DEFINITION('Bonded foot pad (2)','Bonded foot pad (2)',#14676,
#14634);
#14646=PRODUCT_DEFINITION('Bonded foot pad (3)','Bonded foot pad (3)',#14677,
#14634);
#14647=PRODUCT_DEFINITION('Linear Guide Rail - 15 mm, 220 mm Long',
'Linear Guide Rail - 15 mm, 220 mm Long',#14678,#14634);
#14648=PRODUCT_DEFINITION('Slotted Extrusion - 20 x 20 x 200 mm',
'Slotted Extrusion - 20 x 20 x 200 mm',#14679,#14634);
#14649=PRODUCT_DEFINITION('Captive slot nut','Captive slot nut',#14680,
#14634);
#14650=PRODUCT_DEFINITION('M5x14 Cap Screw','M5x14 Cap Screw',#14681,#14634);
#14651=PRODUCT_DEFINITION('M4x10 Cap Screw','M4x10 Cap Screw',#14682,#14634);
#14652=PRODUCT_DEFINITION('Moving table','Moving table',#14683,#14634);
#14653=PRODUCT_DEFINITION('Table plate','Table plate',#14684,#14634);
#14654=PRODUCT_DEFINITION('Bent scale pointer','Bent scale pointer',#14685,
#14634);
#14655=PRODUCT_DEFINITION('Manual grip','Manual grip',#14686,#14634);
#14656=PRODUCT_DEFINITION('Flanged Linear Guide Carriage - 15 mm',
'Flanged Linear Guide Carriage - 15 mm',#14687,#14634);
#14657=PRODUCT_DEFINITION('Block','Block',#14688,#14634);
#14658=PRODUCT_DEFINITION('End cap +','End cap +',#14689,#14634);
#14659=PRODUCT_DEFINITION('End cap','End cap',#14690,#14634);
#14660=PRODUCT_DEFINITION('Flat Washer - M5','Flat Washer - M5',#14691,
#14634);
#14661=PRODUCT_DEFINITION('Cap Screw - M5x20','Cap Screw - M5x20',#14692,
#14634);
#14662=PRODUCT_DEFINITION('Flat Washer - M4','Flat Washer - M4',#14693,
#14634);
#14663=PRODUCT_DEFINITION('Cap Screw - M4x16','Cap Screw - M4x16',#14694,
#14634);
#14664=PRODUCT_DEFINITION('Flat Washer - M6','Flat Washer - M6',#14695,
#14634);
#14665=PRODUCT_DEFINITION('Cap Screw - M6x25','Cap Screw - M6x25',#14696,
#14634);
#14666=PRODUCT_DEFINITION_FORMATION('',$,#14731);
#14667=PRODUCT_DEFINITION_FORMATION('',$,#14732);
#14668=PRODUCT_DEFINITION_FORMATION('',$,#14733);
#14669=PRODUCT_DEFINITION_FORMATION('',$,#14734);
#14670=PRODUCT_DEFINITION_FORMATION('',$,#14735);
#14671=PRODUCT_DEFINITION_FORMATION('',$,#14736);
#14672=PRODUCT_DEFINITION_FORMATION('',$,#14737);
#14673=PRODUCT_DEFINITION_FORMATION('',$,#14738);
#14674=PRODUCT_DEFINITION_FORMATION('',$,#14739);
#14675=PRODUCT_DEFINITION_FORMATION('',$,#14740);
#14676=PRODUCT_DEFINITION_FORMATION('',$,#14741);
#14677=PRODUCT_DEFINITION_FORMATION('',$,#14742);
#14678=PRODUCT_DEFINITION_FORMATION('',$,#14743);
#14679=PRODUCT_DEFINITION_FORMATION('',$,#14744);
#14680=PRODUCT_DEFINITION_FORMATION('',$,#14745);
#14681=PRODUCT_DEFINITION_FORMATION('',$,#14746);
#14682=PRODUCT_DEFINITION_FORMATION('',$,#14747);
#14683=PRODUCT_DEFINITION_FORMATION('',$,#14748);
#14684=PRODUCT_DEFINITION_FORMATION('',$,#14749);
#14685=PRODUCT_DEFINITION_FORMATION('',$,#14750);
#14686=PRODUCT_DEFINITION_FORMATION('',$,#14751);
#14687=PRODUCT_DEFINITION_FORMATION('',$,#14752);
#14688=PRODUCT_DEFINITION_FORMATION('',$,#14753);
#14689=PRODUCT_DEFINITION_FORMATION('',$,#14754);
#14690=PRODUCT_DEFINITION_FORMATION('',$,#14755);
#14691=PRODUCT_DEFINITION_FORMATION('',$,#14756);
#14692=PRODUCT_DEFINITION_FORMATION('',$,#14757);
#14693=PRODUCT_DEFINITION_FORMATION('',$,#14758);
#14694=PRODUCT_DEFINITION_FORMATION('',$,#14759);
#14695=PRODUCT_DEFINITION_FORMATION('',$,#14760);
#14696=PRODUCT_DEFINITION_FORMATION('',$,#14761);
#14697=PRODUCT_RELATED_PRODUCT_CATEGORY('PAT-095','PAT-095',(#14731));
#14698=PRODUCT_RELATED_PRODUCT_CATEGORY('Stationary frame',
'Stationary frame',(#14732));
#14699=PRODUCT_RELATED_PRODUCT_CATEGORY('Base plate','Base plate',(#14733));
#14700=PRODUCT_RELATED_PRODUCT_CATEGORY('End stop','End stop',(#14734));
#14701=PRODUCT_RELATED_PRODUCT_CATEGORY('Bonded stop pad',
'Bonded stop pad',(#14735));
#14702=PRODUCT_RELATED_PRODUCT_CATEGORY('End stop (1)','End stop (1)',(#14736));
#14703=PRODUCT_RELATED_PRODUCT_CATEGORY('Bonded stop pad (1)',
'Bonded stop pad (1)',(#14737));
#14704=PRODUCT_RELATED_PRODUCT_CATEGORY('Graduated scale',
'Graduated scale',(#14738));
#14705=PRODUCT_RELATED_PRODUCT_CATEGORY('Bonded foot pad',
'Bonded foot pad',(#14739));
#14706=PRODUCT_RELATED_PRODUCT_CATEGORY('Bonded foot pad (1)',
'Bonded foot pad (1)',(#14740));
#14707=PRODUCT_RELATED_PRODUCT_CATEGORY('Bonded foot pad (2)',
'Bonded foot pad (2)',(#14741));
#14708=PRODUCT_RELATED_PRODUCT_CATEGORY('Bonded foot pad (3)',
'Bonded foot pad (3)',(#14742));
#14709=PRODUCT_RELATED_PRODUCT_CATEGORY(
'Linear Guide Rail - 15 mm, 220 mm Long',
'Linear Guide Rail - 15 mm, 220 mm Long',(#14743));
#14710=PRODUCT_RELATED_PRODUCT_CATEGORY(
'Slotted Extrusion - 20 x 20 x 200 mm',
'Slotted Extrusion - 20 x 20 x 200 mm',(#14744));
#14711=PRODUCT_RELATED_PRODUCT_CATEGORY('Captive slot nut',
'Captive slot nut',(#14745));
#14712=PRODUCT_RELATED_PRODUCT_CATEGORY('M5x14 Cap Screw',
'M5x14 Cap Screw',(#14746));
#14713=PRODUCT_RELATED_PRODUCT_CATEGORY('M4x10 Cap Screw',
'M4x10 Cap Screw',(#14747));
#14714=PRODUCT_RELATED_PRODUCT_CATEGORY('Moving table','Moving table',(#14748));
#14715=PRODUCT_RELATED_PRODUCT_CATEGORY('Table plate','Table plate',(#14749));
#14716=PRODUCT_RELATED_PRODUCT_CATEGORY('Bent scale pointer',
'Bent scale pointer',(#14750));
#14717=PRODUCT_RELATED_PRODUCT_CATEGORY('Manual grip','Manual grip',(#14751));
#14718=PRODUCT_RELATED_PRODUCT_CATEGORY(
'Flanged Linear Guide Carriage - 15 mm',
'Flanged Linear Guide Carriage - 15 mm',(#14752));
#14719=PRODUCT_RELATED_PRODUCT_CATEGORY('Block','Block',(#14753));
#14720=PRODUCT_RELATED_PRODUCT_CATEGORY('End cap +','End cap +',(#14754));
#14721=PRODUCT_RELATED_PRODUCT_CATEGORY('End cap','End cap',(#14755));
#14722=PRODUCT_RELATED_PRODUCT_CATEGORY('Flat Washer - M5',
'Flat Washer - M5',(#14756));
#14723=PRODUCT_RELATED_PRODUCT_CATEGORY('Cap Screw - M5x20',
'Cap Screw - M5x20',(#14757));
#14724=PRODUCT_RELATED_PRODUCT_CATEGORY('Flat Washer - M4',
'Flat Washer - M4',(#14758));
#14725=PRODUCT_RELATED_PRODUCT_CATEGORY('Cap Screw - M4x16',
'Cap Screw - M4x16',(#14759));
#14726=PRODUCT_RELATED_PRODUCT_CATEGORY('Flat Washer - M6',
'Flat Washer - M6',(#14760));
#14727=PRODUCT_RELATED_PRODUCT_CATEGORY('Cap Screw - M6x25',
'Cap Screw - M6x25',(#14761));
#14728=APPLICATION_PROTOCOL_DEFINITION('international standard',
'automotive_design',2009,#14729);
#14729=APPLICATION_CONTEXT(
'Core Data for Automotive Mechanical Design Process');
#14730=PRODUCT_CONTEXT('part definition',#14729,'mechanical');
#14731=PRODUCT('PAT-095','PAT-095',
'PAT-095',(#14730));
#14732=PRODUCT('Stationary frame','Stationary frame','Stationary frame',
(#14730));
#14733=PRODUCT('Base plate','Base plate','Base plate',(#14730));
#14734=PRODUCT('End stop','End stop','End stop',(#14730));
#14735=PRODUCT('Bonded stop pad','Bonded stop pad','Bonded stop pad',(#14730));
#14736=PRODUCT('End stop (1)','End stop (1)','End stop (1)',(#14730));
#14737=PRODUCT('Bonded stop pad (1)','Bonded stop pad (1)',
'Bonded stop pad (1)',(#14730));
#14738=PRODUCT('Graduated scale','Graduated scale','Graduated scale',(#14730));
#14739=PRODUCT('Bonded foot pad','Bonded foot pad','Bonded foot pad',(#14730));
#14740=PRODUCT('Bonded foot pad (1)','Bonded foot pad (1)',
'Bonded foot pad (1)',(#14730));
#14741=PRODUCT('Bonded foot pad (2)','Bonded foot pad (2)',
'Bonded foot pad (2)',(#14730));
#14742=PRODUCT('Bonded foot pad (3)','Bonded foot pad (3)',
'Bonded foot pad (3)',(#14730));
#14743=PRODUCT('Linear Guide Rail - 15 mm, 220 mm Long',
'Linear Guide Rail - 15 mm, 220 mm Long',
'Linear Guide Rail - 15 mm, 220 mm Long',(#14730));
#14744=PRODUCT('Slotted Extrusion - 20 x 20 x 200 mm',
'Slotted Extrusion - 20 x 20 x 200 mm',
'Slotted Extrusion - 20 x 20 x 200 mm',(#14730));
#14745=PRODUCT('Captive slot nut','Captive slot nut','Captive slot nut',
(#14730));
#14746=PRODUCT('M5x14 Cap Screw','M5x14 Cap Screw','M5x14 Cap Screw',(#14730));
#14747=PRODUCT('M4x10 Cap Screw','M4x10 Cap Screw','M4x10 Cap Screw',(#14730));
#14748=PRODUCT('Moving table','Moving table','Moving table',(#14730));
#14749=PRODUCT('Table plate','Table plate','Table plate',(#14730));
#14750=PRODUCT('Bent scale pointer','Bent scale pointer',
'Bent scale pointer',(#14730));
#14751=PRODUCT('Manual grip','Manual grip','Manual grip',(#14730));
#14752=PRODUCT('Flanged Linear Guide Carriage - 15 mm',
'Flanged Linear Guide Carriage - 15 mm',
'Flanged Linear Guide Carriage - 15 mm',(#14730));
#14753=PRODUCT('Block','Block','Block',(#14730));
#14754=PRODUCT('End cap +','End cap +','End cap +',(#14730));
#14755=PRODUCT('End cap','End cap','End cap',(#14730));
#14756=PRODUCT('Flat Washer - M5','Flat Washer - M5','Flat Washer - M5',
(#14730));
#14757=PRODUCT('Cap Screw - M5x20','Cap Screw - M5x20',
'Cap Screw - M5x20',(#14730));
#14758=PRODUCT('Flat Washer - M4','Flat Washer - M4','Flat Washer - M4',
(#14730));
#14759=PRODUCT('Cap Screw - M4x16','Cap Screw - M4x16',
'Cap Screw - M4x16',(#14730));
#14760=PRODUCT('Flat Washer - M6','Flat Washer - M6','Flat Washer - M6',
(#14730));
#14761=PRODUCT('Cap Screw - M6x25','Cap Screw - M6x25',
'Cap Screw - M6x25',(#14730));
#14762=PRESENTATION_STYLE_ASSIGNMENT((#14768));
#14763=PRESENTATION_STYLE_ASSIGNMENT((#14769));
#14764=PRESENTATION_STYLE_ASSIGNMENT((#14770));
#14765=PRESENTATION_STYLE_ASSIGNMENT((#14771));
#14766=PRESENTATION_STYLE_ASSIGNMENT((#14772));
#14767=PRESENTATION_STYLE_ASSIGNMENT((#14773));
#14768=SURFACE_STYLE_USAGE(.BOTH.,#14774);
#14769=SURFACE_STYLE_USAGE(.BOTH.,#14775);
#14770=SURFACE_STYLE_USAGE(.BOTH.,#14776);
#14771=SURFACE_STYLE_USAGE(.BOTH.,#14777);
#14772=SURFACE_STYLE_USAGE(.BOTH.,#14778);
#14773=SURFACE_STYLE_USAGE(.BOTH.,#14779);
#14774=SURFACE_SIDE_STYLE('',(#14780));
#14775=SURFACE_SIDE_STYLE('',(#14781));
#14776=SURFACE_SIDE_STYLE('',(#14782));
#14777=SURFACE_SIDE_STYLE('',(#14783));
#14778=SURFACE_SIDE_STYLE('',(#14784));
#14779=SURFACE_SIDE_STYLE('',(#14785));
#14780=SURFACE_STYLE_FILL_AREA(#14786);
#14781=SURFACE_STYLE_FILL_AREA(#14787);
#14782=SURFACE_STYLE_FILL_AREA(#14788);
#14783=SURFACE_STYLE_FILL_AREA(#14789);
#14784=SURFACE_STYLE_FILL_AREA(#14790);
#14785=SURFACE_STYLE_FILL_AREA(#14791);
#14786=FILL_AREA_STYLE('Steel - Satin',(#14792));
#14787=FILL_AREA_STYLE('CAD Library Painted - Deep blue',(#14793));
#14788=FILL_AREA_STYLE('CAD Library Painted - Engineering blue',(#14794));
#14789=FILL_AREA_STYLE('CAD Library Painted - Graphite',(#14795));
#14790=FILL_AREA_STYLE('CAD Library Painted - Steel gray',(#14796));
#14791=FILL_AREA_STYLE('CAD Library Painted - Light blue',(#14797));
#14792=FILL_AREA_STYLE_COLOUR('Steel - Satin',#14798);
#14793=FILL_AREA_STYLE_COLOUR('CAD Library Painted - Deep blue',#14799);
#14794=FILL_AREA_STYLE_COLOUR('CAD Library Painted - Engineering blue',
#14800);
#14795=FILL_AREA_STYLE_COLOUR('CAD Library Painted - Graphite',#14801);
#14796=FILL_AREA_STYLE_COLOUR('CAD Library Painted - Steel gray',#14802);
#14797=FILL_AREA_STYLE_COLOUR('CAD Library Painted - Light blue',#14803);
#14798=COLOUR_RGB('Steel - Satin',0.627450980392157,0.627450980392157,0.627450980392157);
#14799=COLOUR_RGB('CAD Library Painted - Deep blue',0.0784313725490196,
0.203921568627451,0.349019607843137);
#14800=COLOUR_RGB('CAD Library Painted - Engineering blue',0.12156862745098,
0.356862745098039,0.6);
#14801=COLOUR_RGB('CAD Library Painted - Graphite',0.168627450980392,0.192156862745098,
0.231372549019608);
#14802=COLOUR_RGB('CAD Library Painted - Steel gray',0.592156862745098,
0.631372549019608,0.67843137254902);
#14803=COLOUR_RGB('CAD Library Painted - Light blue',0.286274509803922,
0.552941176470588,0.780392156862745);
#14804=COLOUR_RGB('Dark Blue',0.08,0.2,0.34);
#14805=FILL_AREA_STYLE_COLOUR('',#14804);
#14806=FILL_AREA_STYLE('',(#14805));
#14807=SURFACE_STYLE_FILL_AREA(#14806);
#14808=SURFACE_SIDE_STYLE('',(#14807));
#14809=SURFACE_STYLE_USAGE(.BOTH.,#14808);
#14810=PRESENTATION_STYLE_ASSIGNMENT((#14809));
#14811=COLOUR_RGB('Light Blue',0.38,0.62,0.78);
#14812=FILL_AREA_STYLE_COLOUR('',#14811);
#14813=FILL_AREA_STYLE('',(#14812));
#14814=SURFACE_STYLE_FILL_AREA(#14813);
#14815=SURFACE_SIDE_STYLE('',(#14814));
#14816=SURFACE_STYLE_USAGE(.BOTH.,#14815);
#14817=PRESENTATION_STYLE_ASSIGNMENT((#14816));
#14818=COLOUR_RGB('Sky Blue',0.24,0.69,0.87);
#14819=FILL_AREA_STYLE_COLOUR('',#14818);
#14820=FILL_AREA_STYLE('',(#14819));
#14821=SURFACE_STYLE_FILL_AREA(#14820);
#14822=SURFACE_SIDE_STYLE('',(#14821));
#14823=SURFACE_STYLE_USAGE(.BOTH.,#14822);
#14824=PRESENTATION_STYLE_ASSIGNMENT((#14823));
#14825=COLOUR_RGB('Grey',0.48,0.52,0.57);
#14826=FILL_AREA_STYLE_COLOUR('',#14825);
#14827=FILL_AREA_STYLE('',(#14826));
#14828=SURFACE_STYLE_FILL_AREA(#14827);
#14829=SURFACE_SIDE_STYLE('',(#14828));
#14830=SURFACE_STYLE_USAGE(.BOTH.,#14829);
#14831=PRESENTATION_STYLE_ASSIGNMENT((#14830));
#14832=COLOUR_RGB('Black',0.12,0.14,0.17);
#14833=FILL_AREA_STYLE_COLOUR('',#14832);
#14834=FILL_AREA_STYLE('',(#14833));
#14835=SURFACE_STYLE_FILL_AREA(#14834);
#14836=SURFACE_SIDE_STYLE('',(#14835));
#14837=SURFACE_STYLE_USAGE(.BOTH.,#14836);
#14838=PRESENTATION_STYLE_ASSIGNMENT((#14837));
#14839=COLOUR_RGB('Off White',0.89,0.88,0.83);
#14840=FILL_AREA_STYLE_COLOUR('',#14839);
#14841=FILL_AREA_STYLE('',(#14840));
#14842=SURFACE_STYLE_FILL_AREA(#14841);
#14843=SURFACE_SIDE_STYLE('',(#14842));
#14844=SURFACE_STYLE_USAGE(.BOTH.,#14843);
#14845=PRESENTATION_STYLE_ASSIGNMENT((#14844));
ENDSEC;
END-ISO-10303-21;
